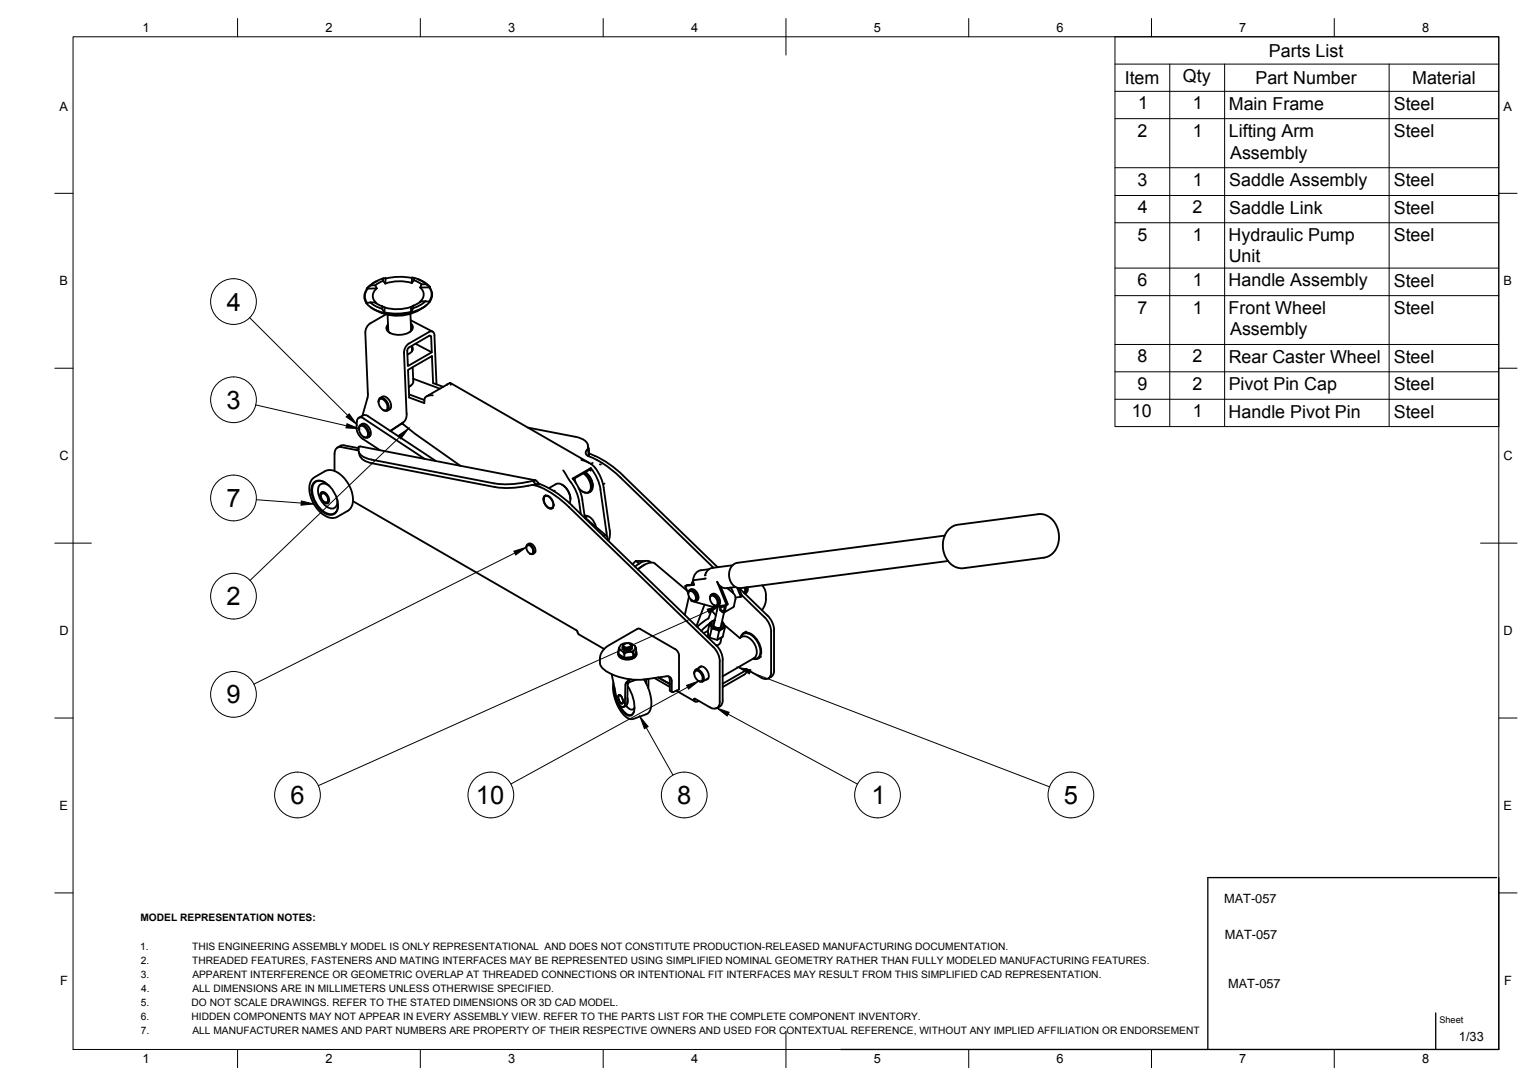
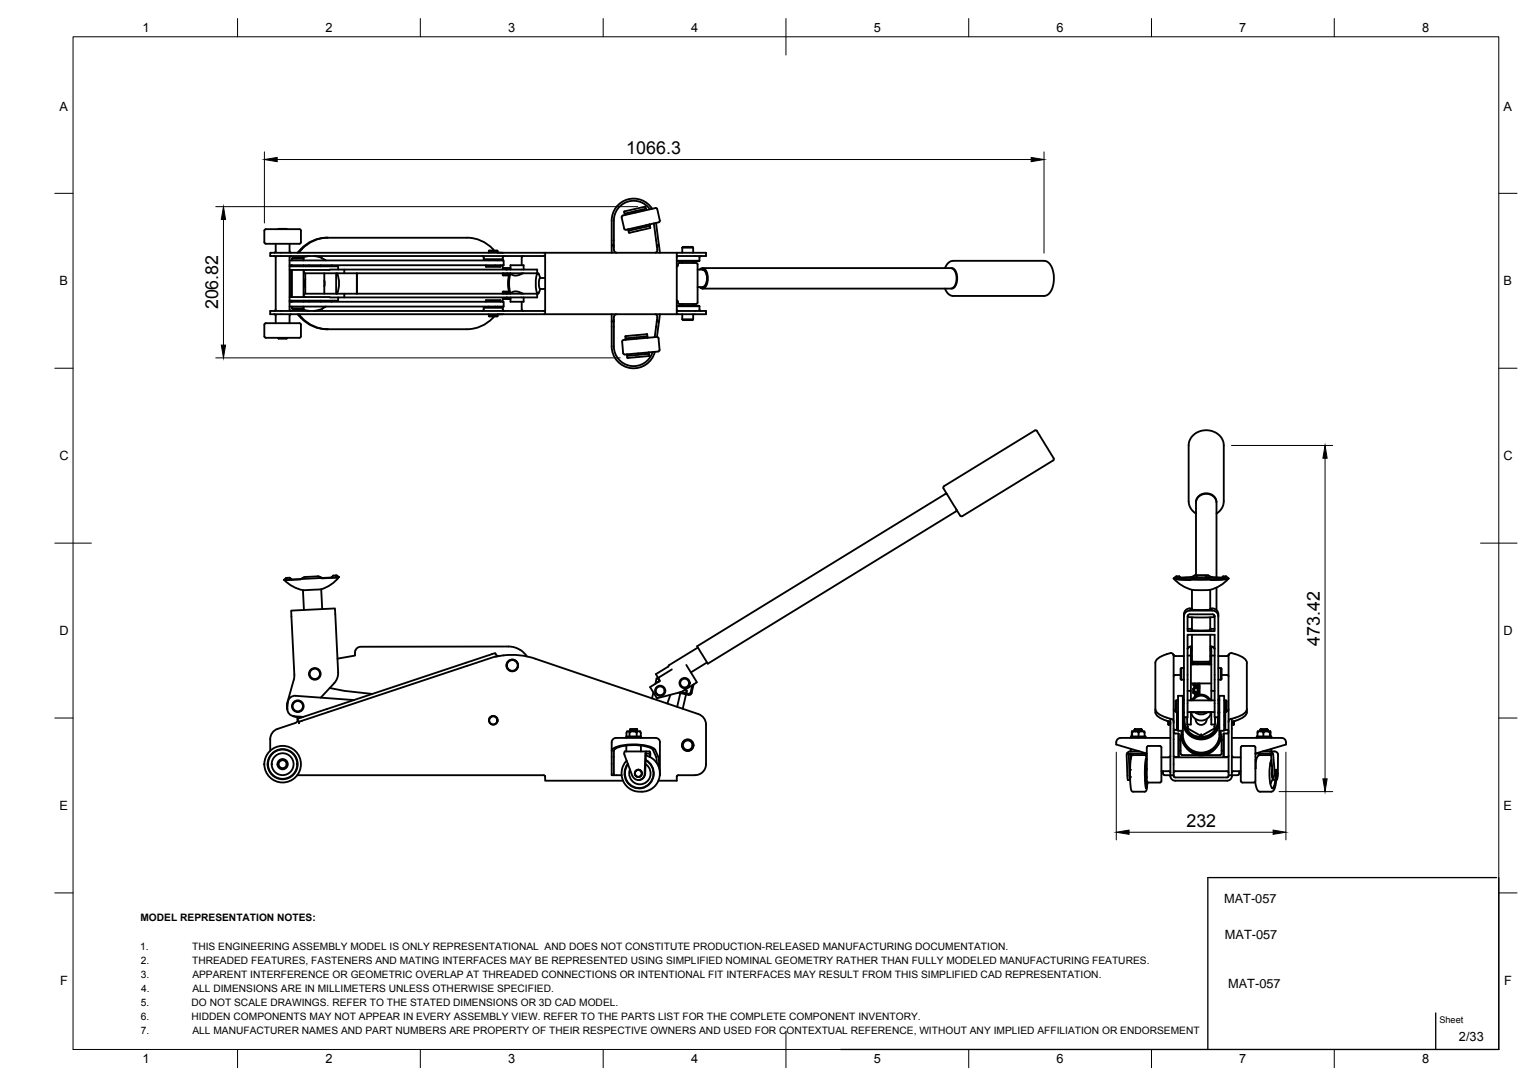
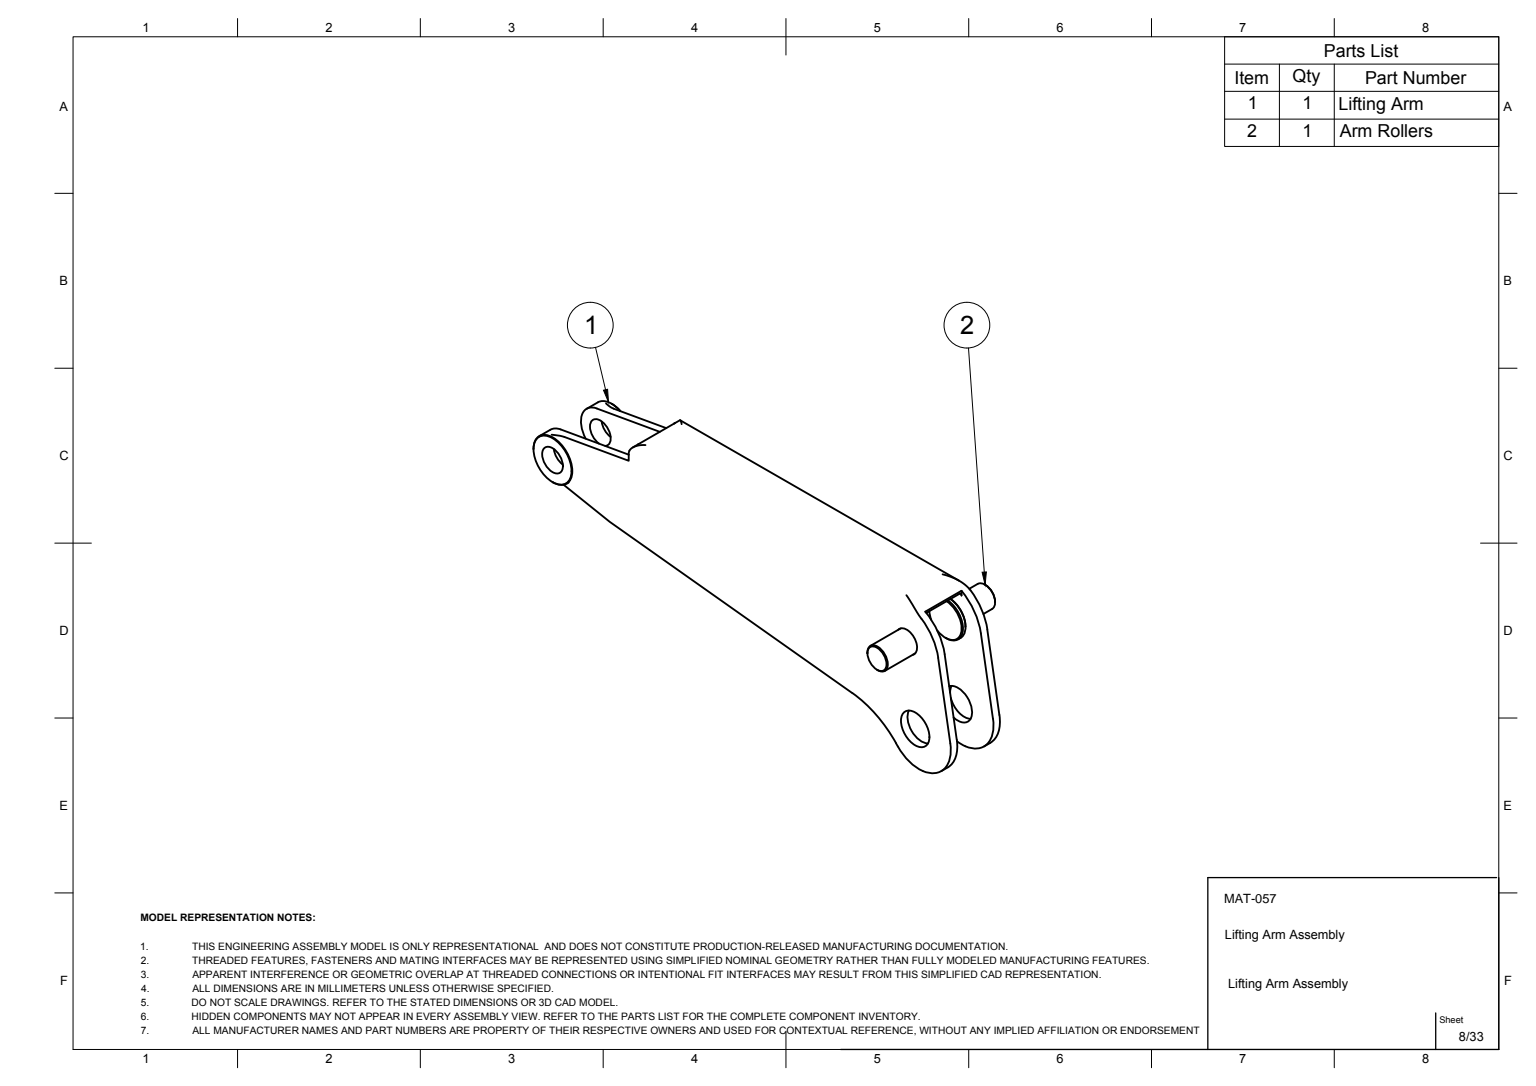
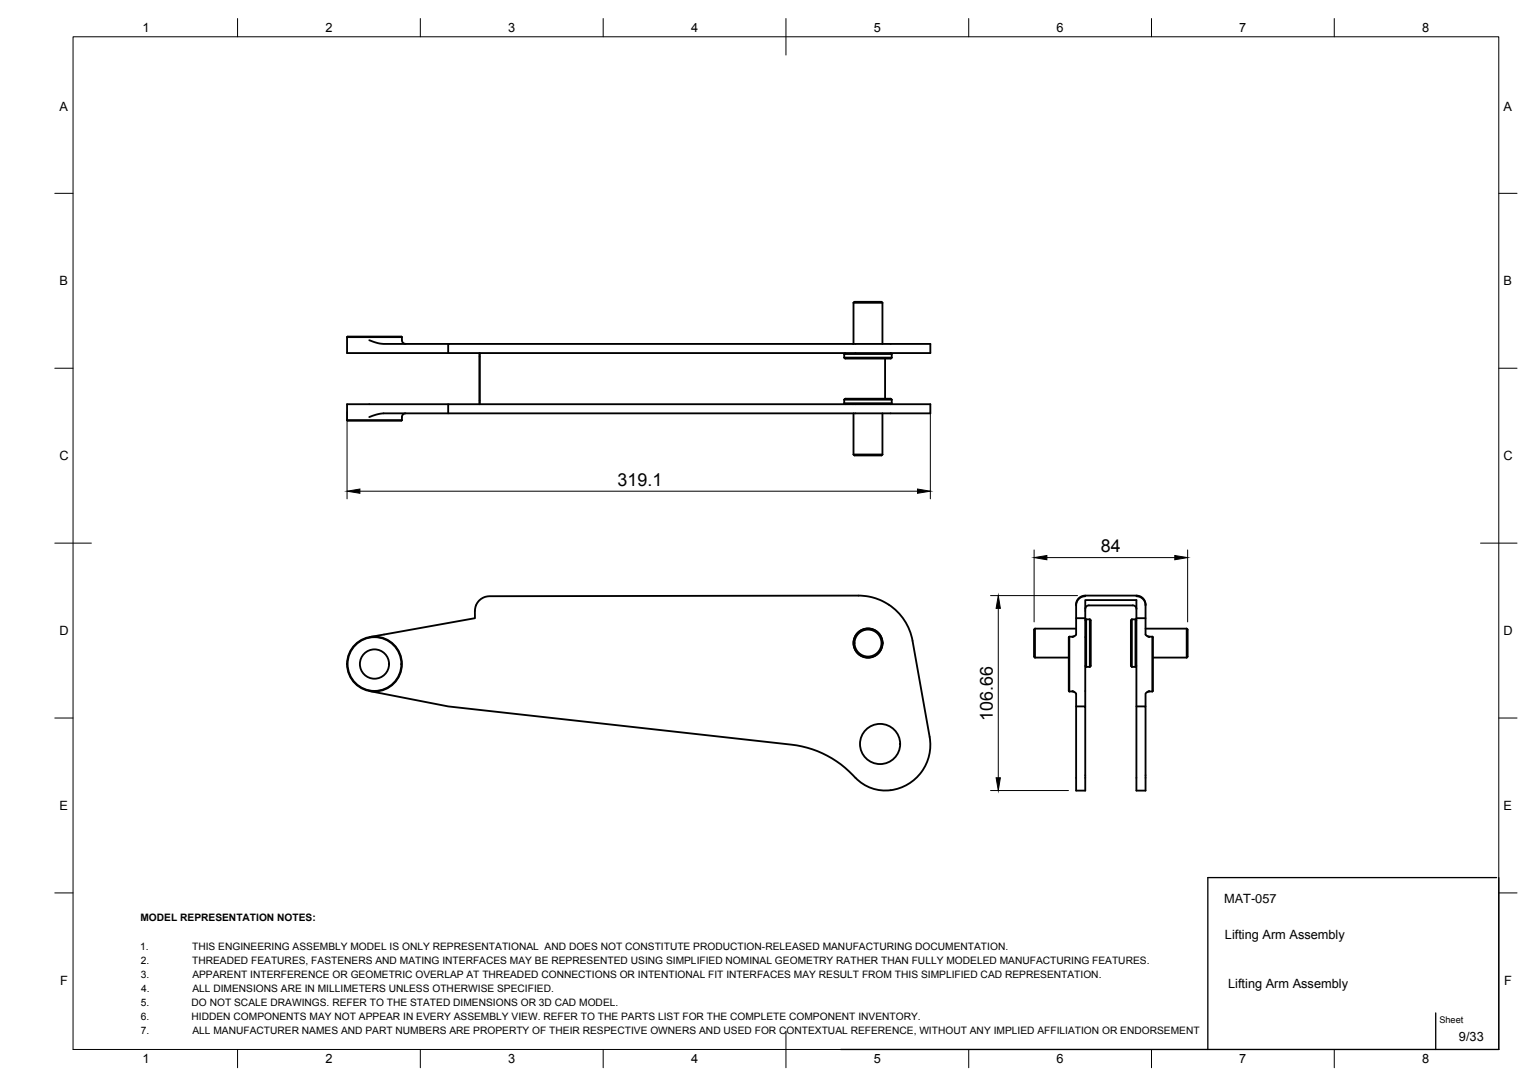
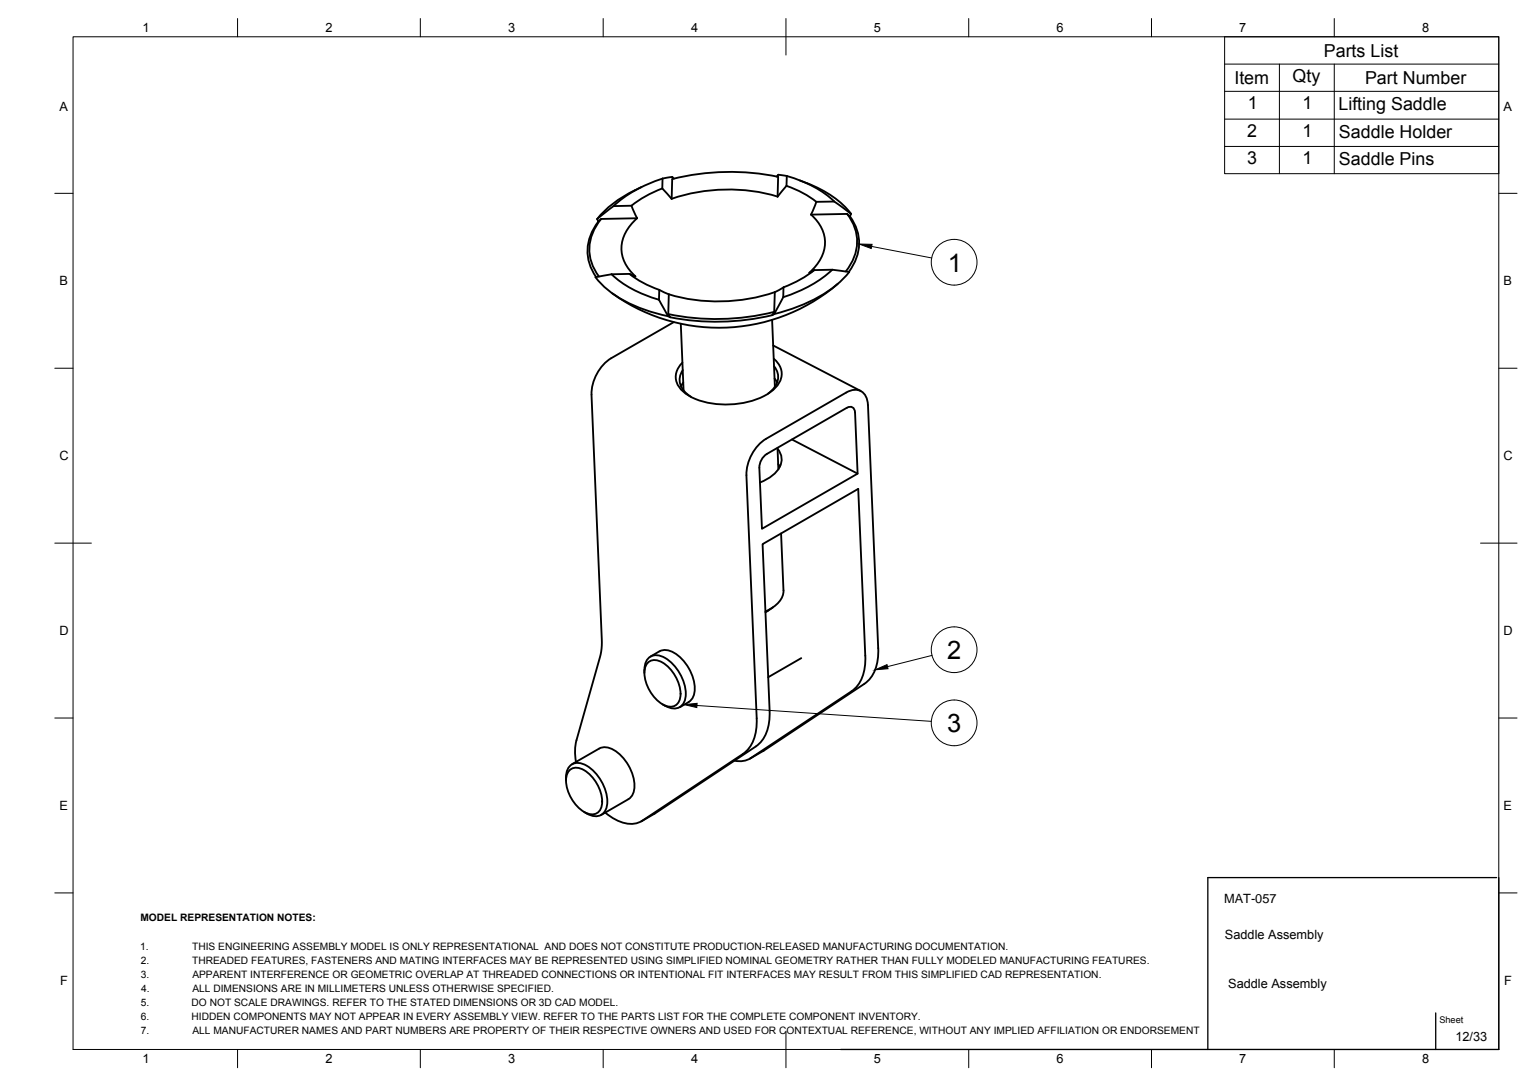
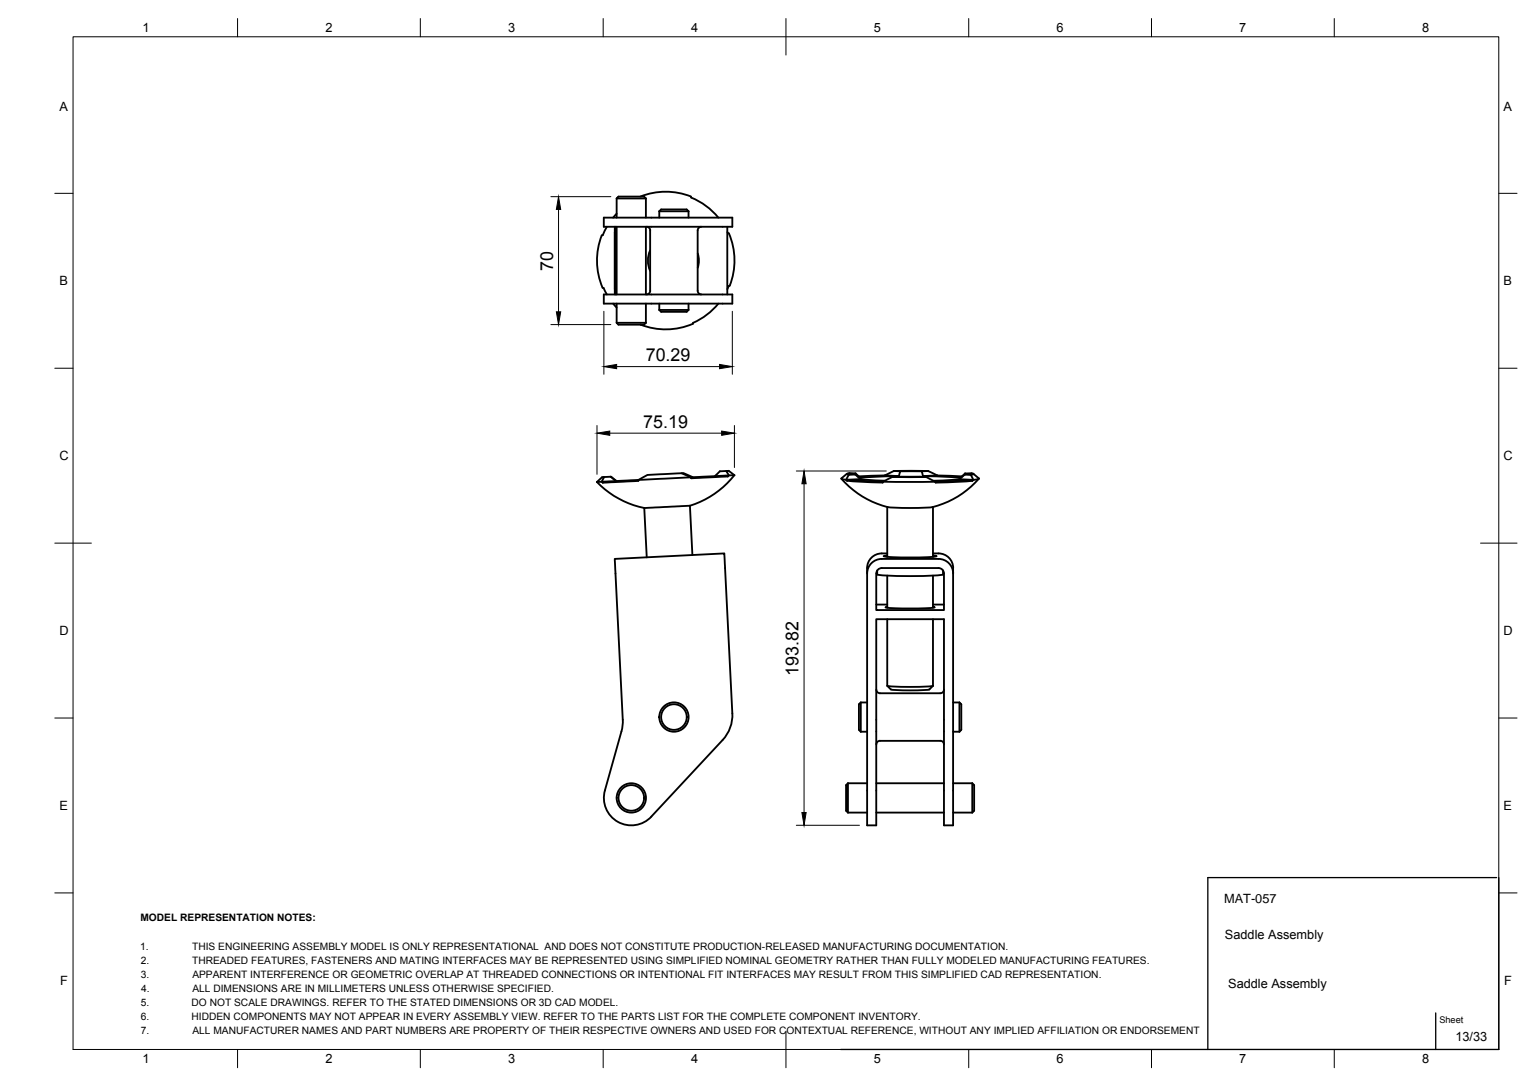
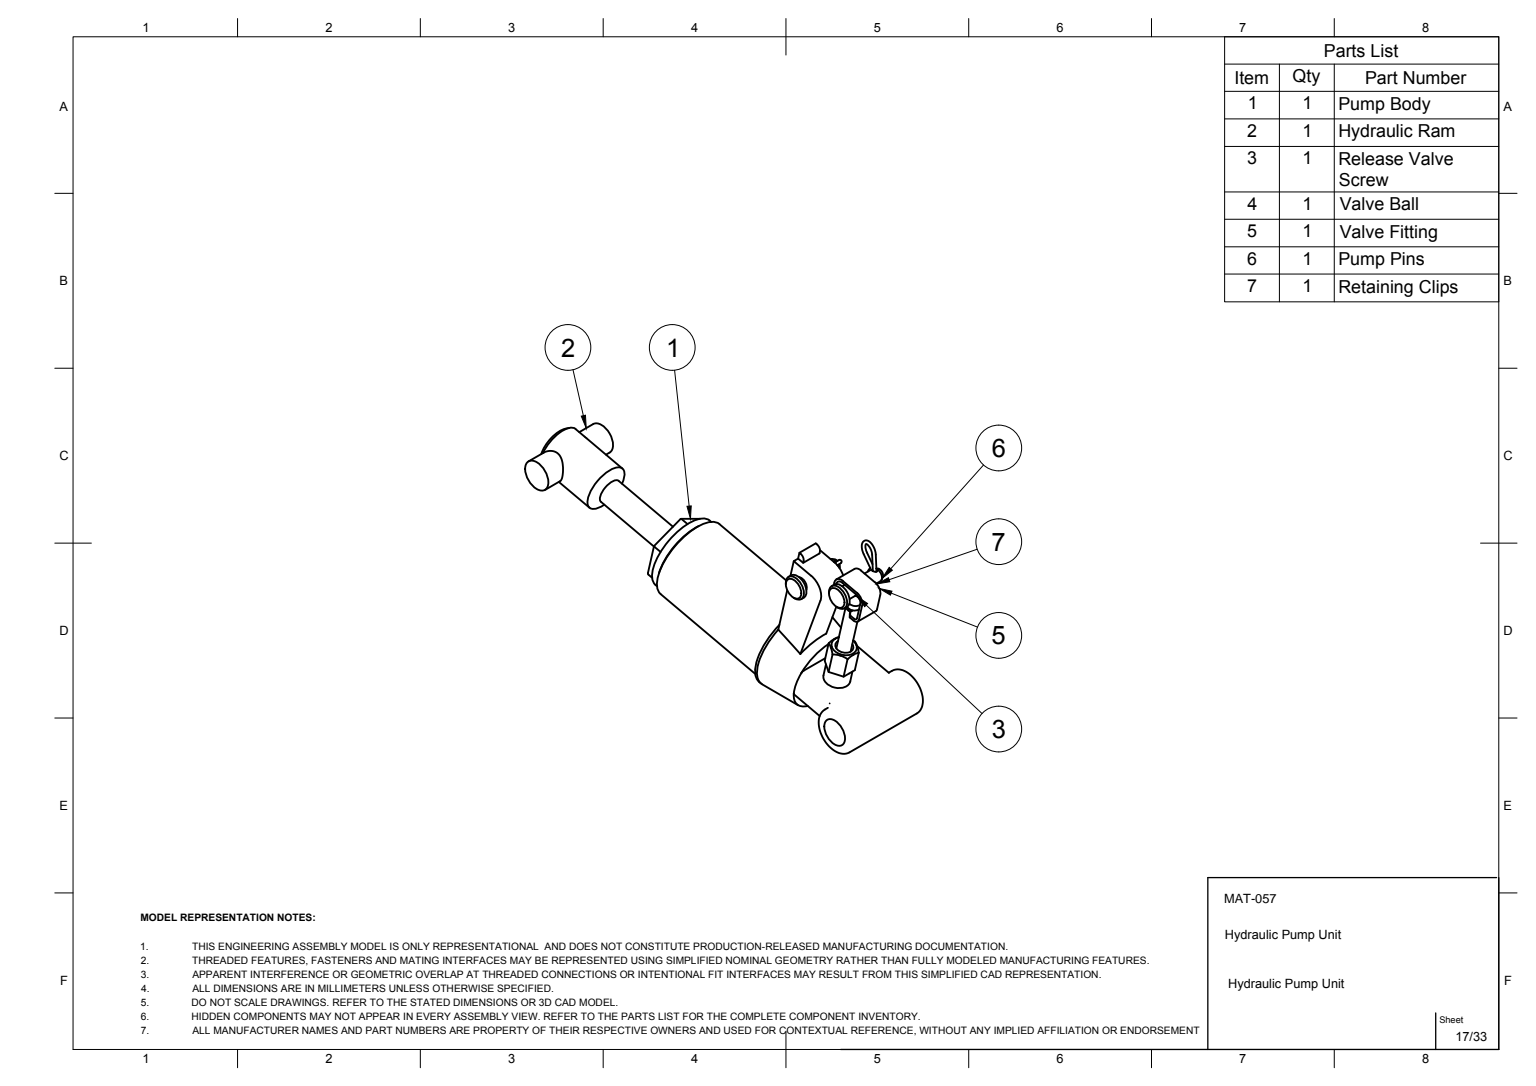
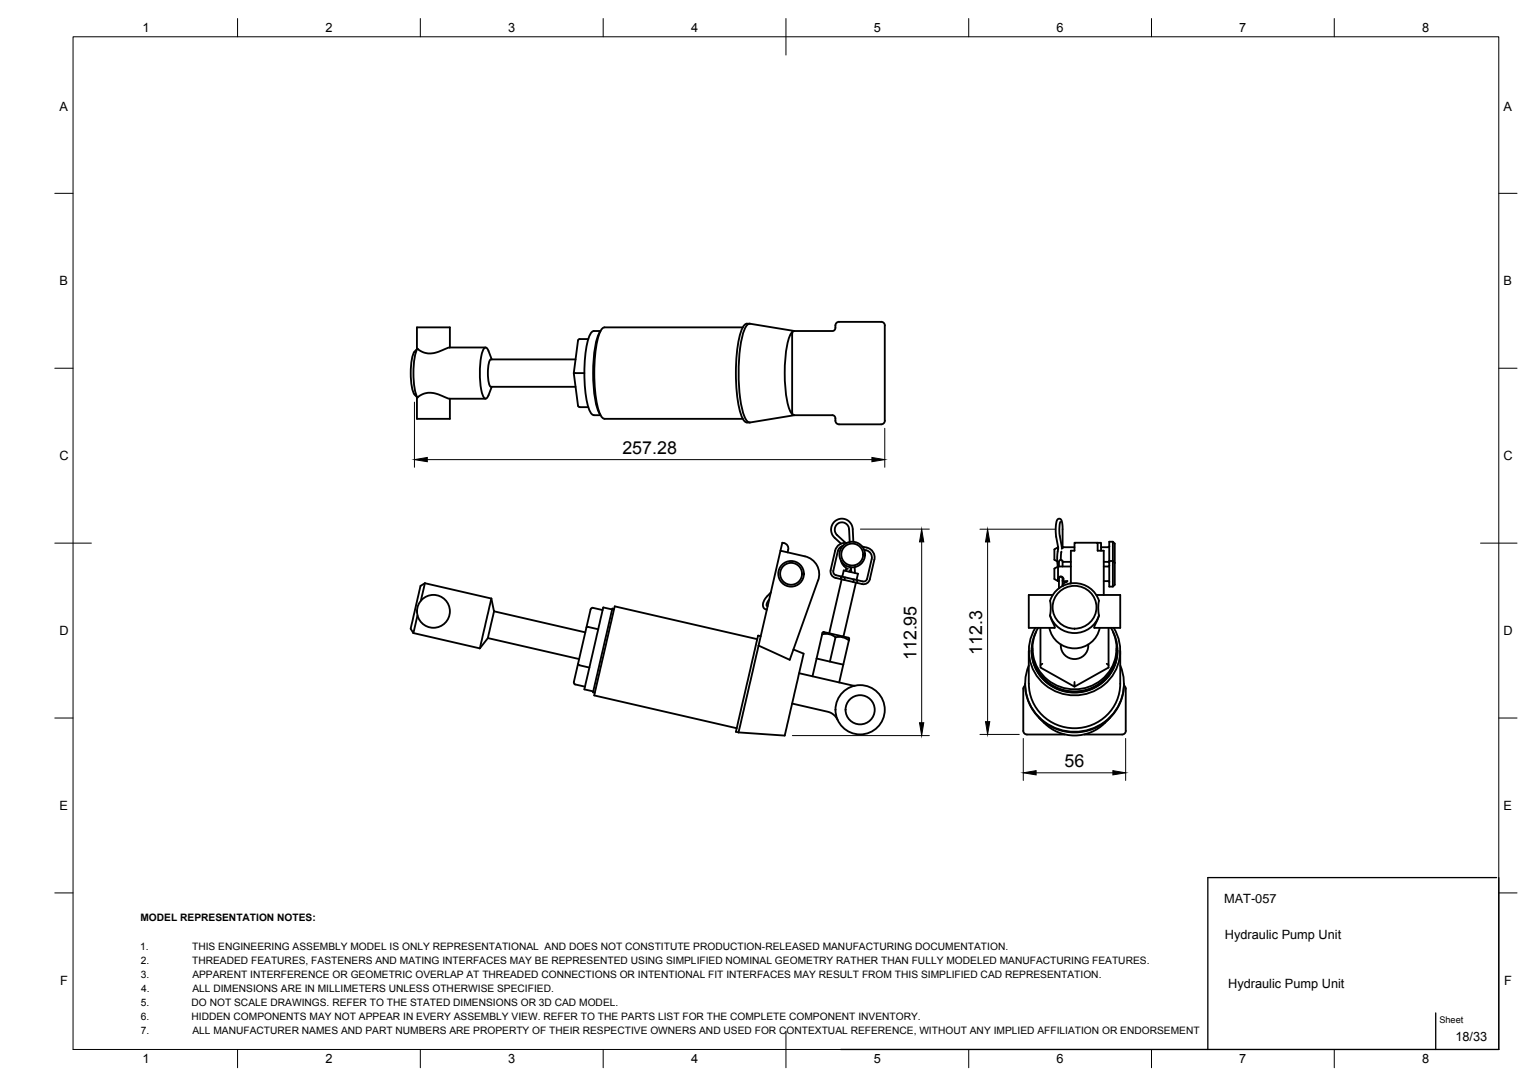
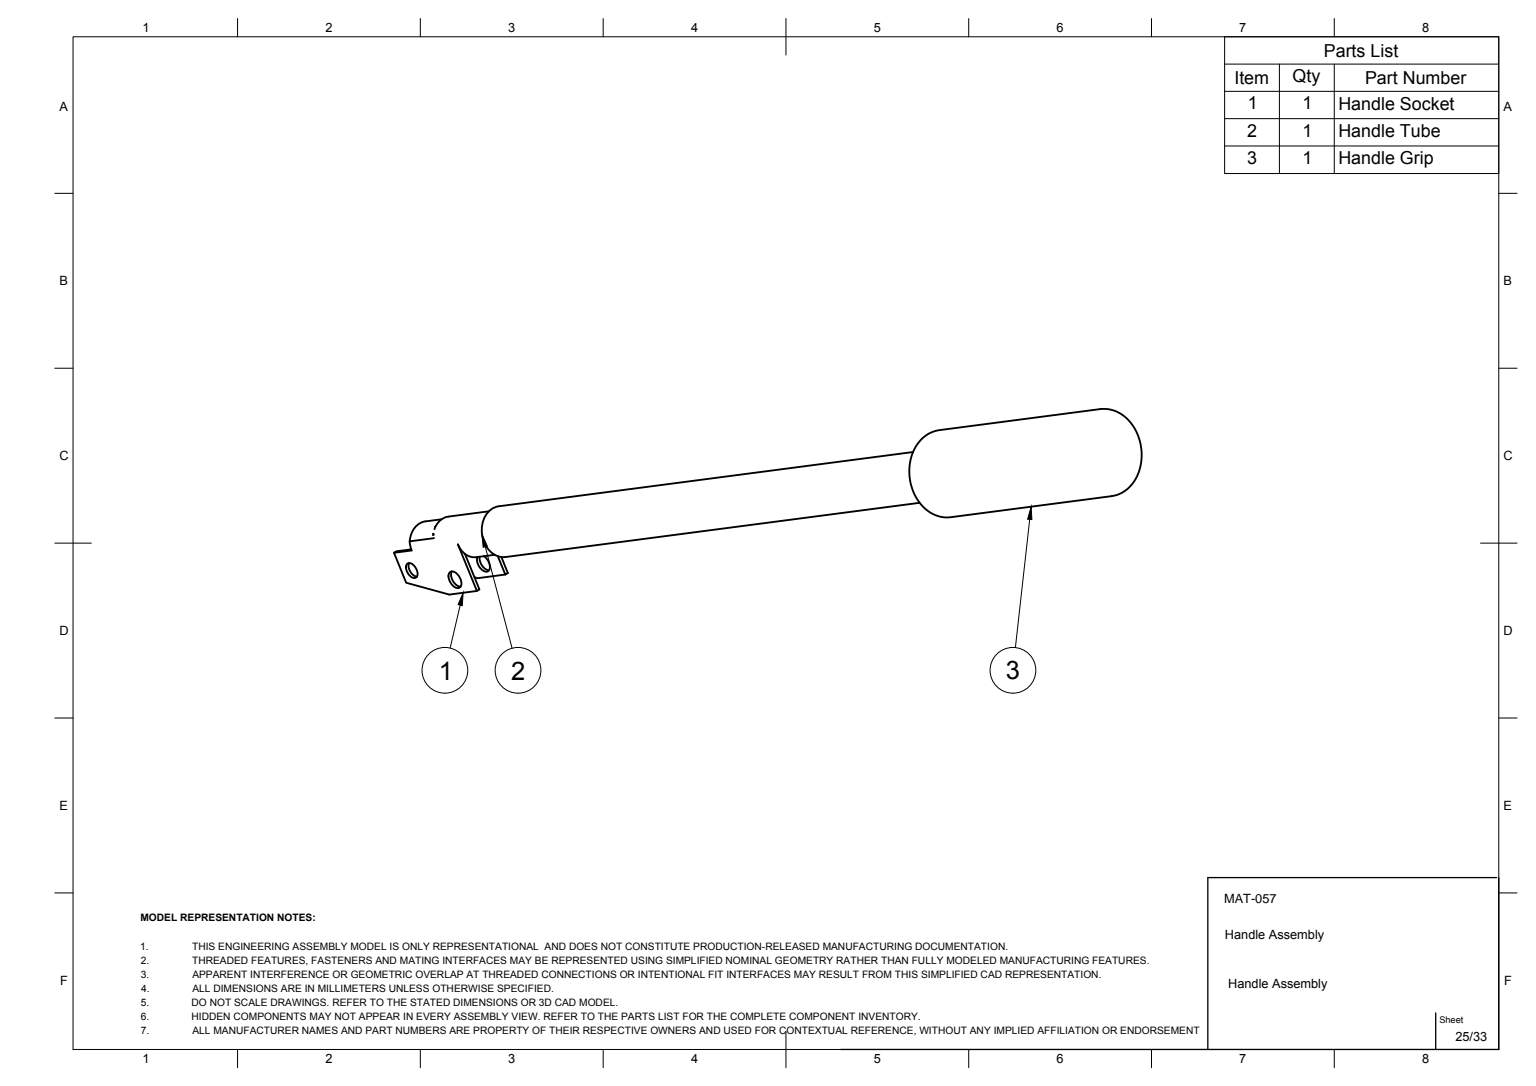
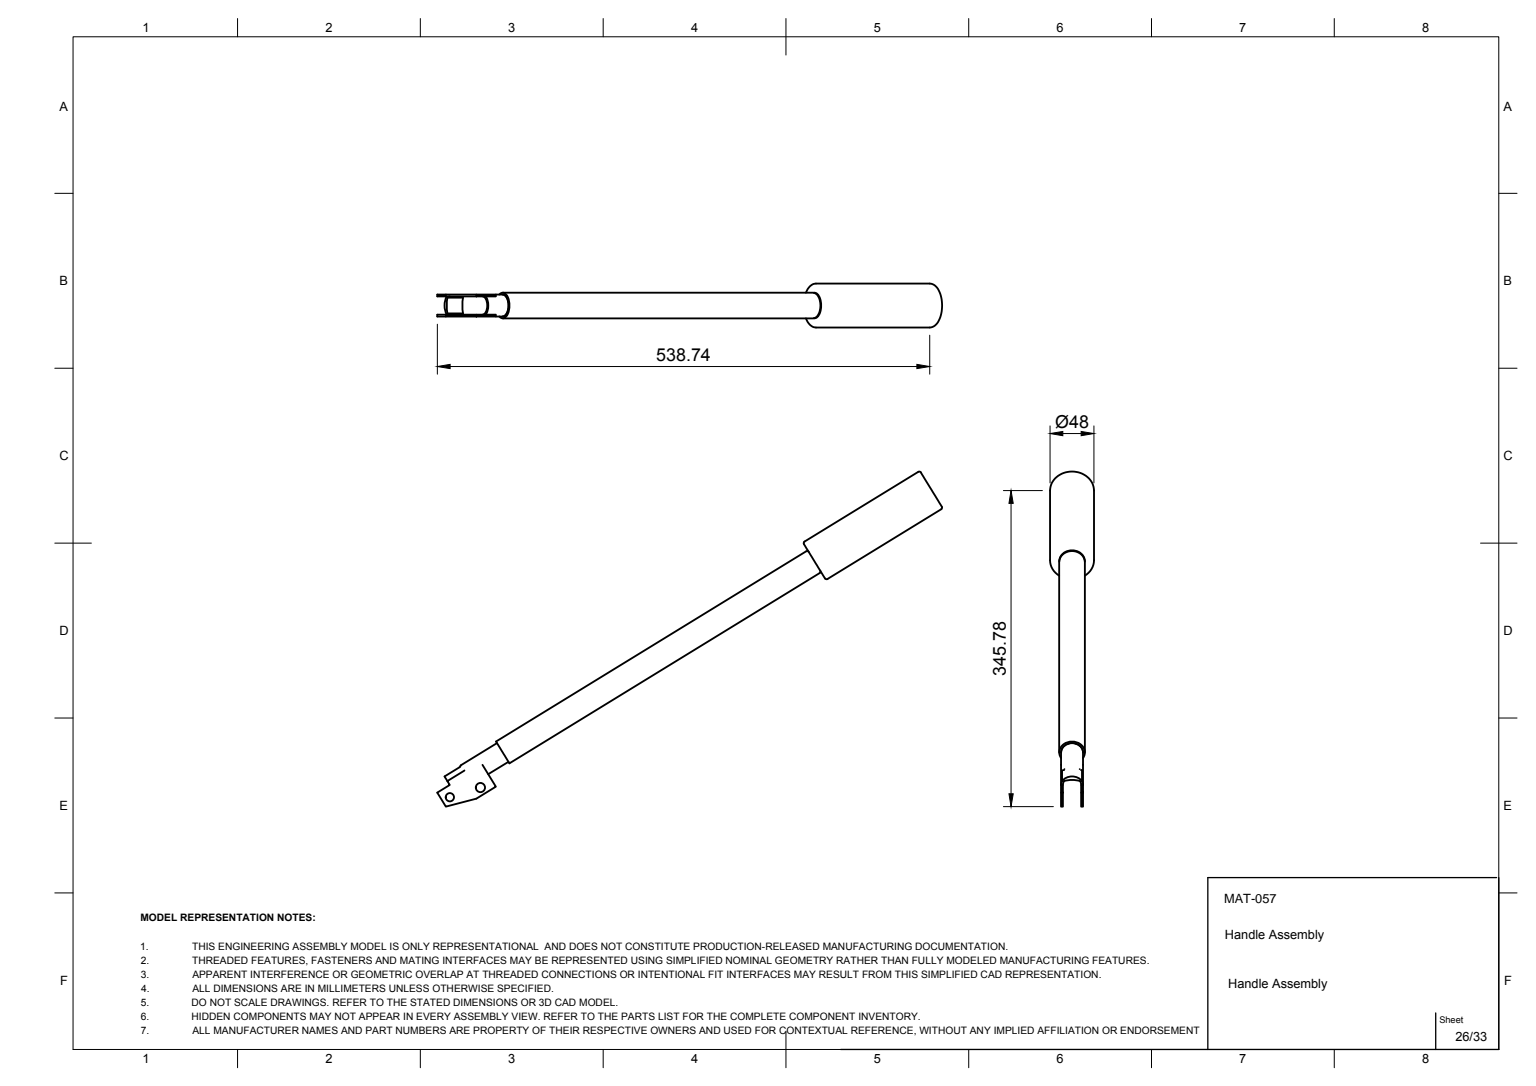
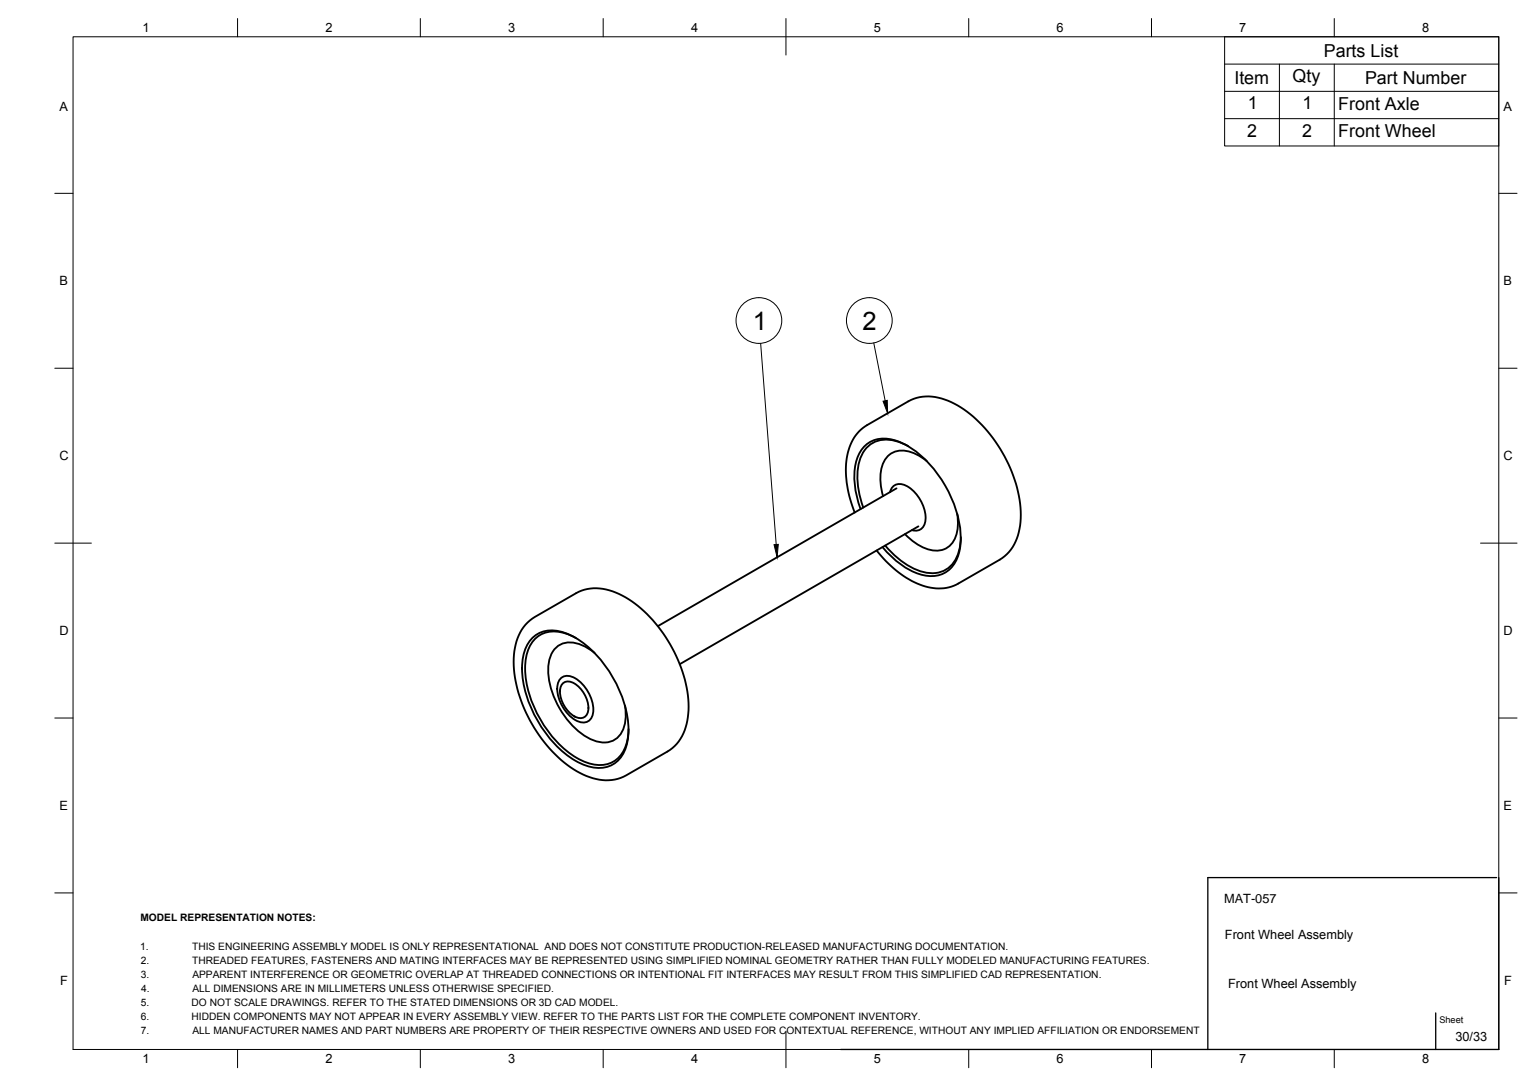
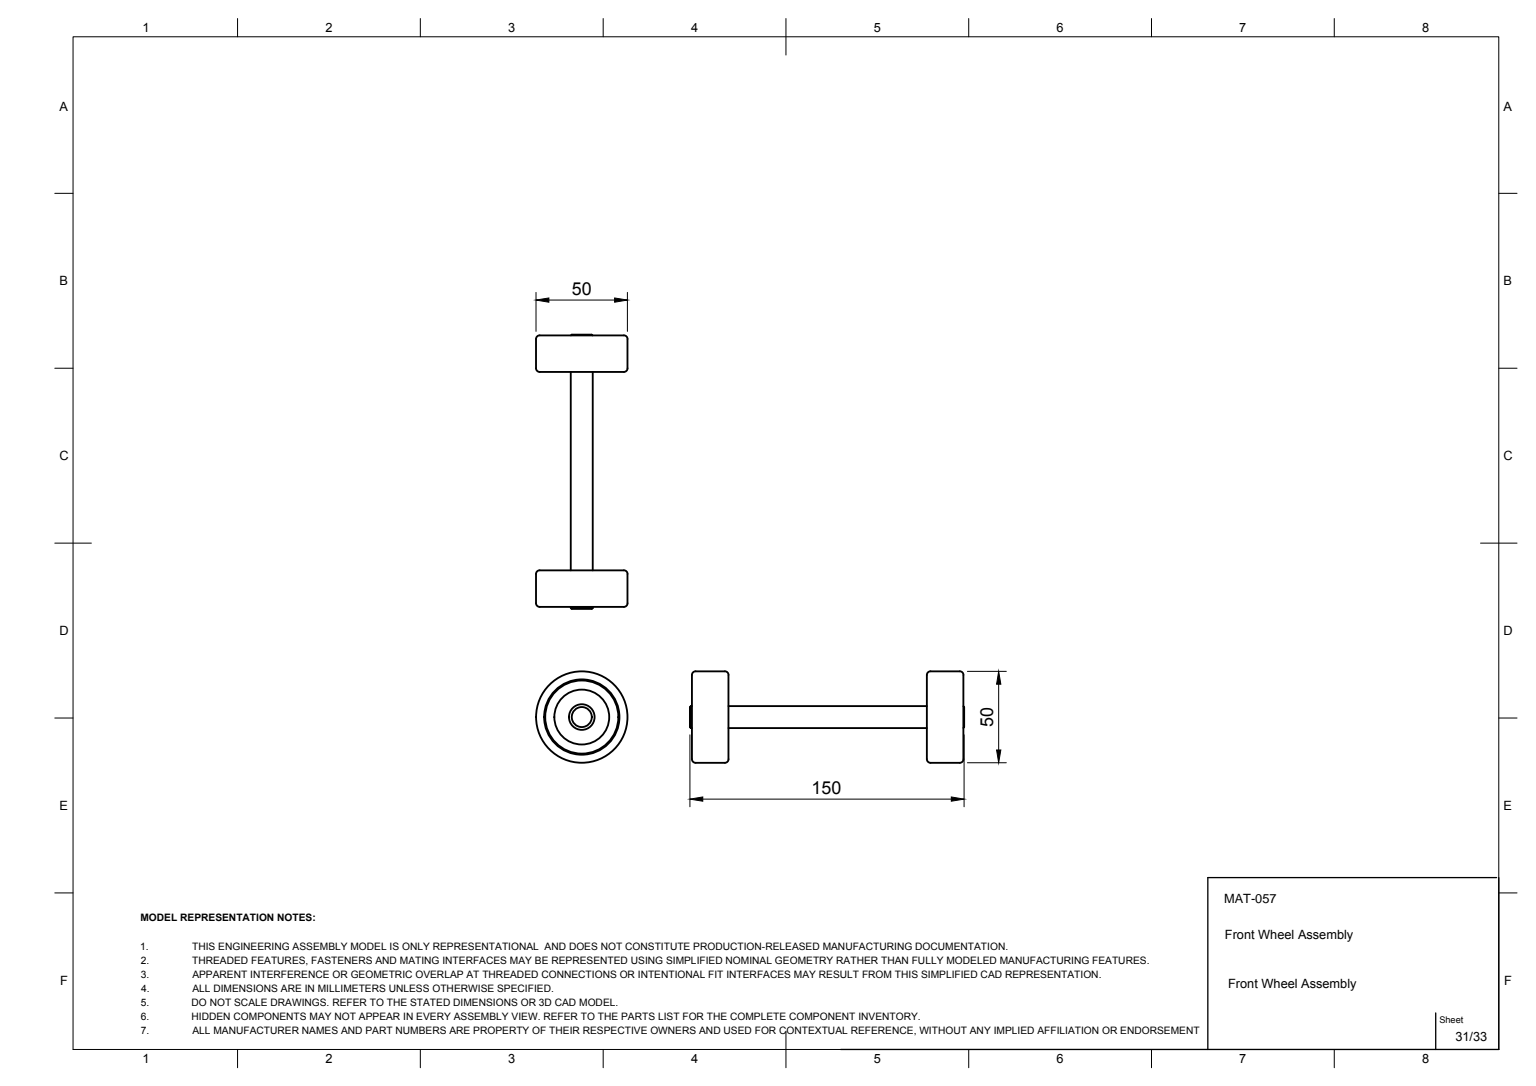
ISO-10303-21;
HEADER;
/* Generated by software containing ST-Developer
 * from STEP Tools, Inc. (www.steptools.com) 
 */

FILE_DESCRIPTION(
/* description */ ('STEP AP214', 'CAx-IF Rec.Pracs.---Representation and Presentation of Product Manufa
cturing Information (PMI)---4.0---2014-10-13'),
/* implementation_level */ '2;1');

FILE_NAME(
/* name */ 'MAT-057',
/* time_stamp */ '2026-10-28T23:34:22+01:00',
/* author */ (''),
/* organization */ (''),
/* preprocessor_version */ 'ST-DEVELOPER v20.2',
/* originating_system */ 'Autodesk Translation Framework v15.17.0.0',
/* authorisation */ '');

FILE_SCHEMA (('AP242_MANAGED_MODEL_BASED_3D_ENGINEERING_MIM_LF { 1 0 10303 442 2 1 4 }'));
ENDSEC;

DATA;
#10=MECHANICAL_DESIGN_GEOMETRIC_PRESENTATION_REPRESENTATION('',(#250,#251,
#252,#253,#254,#255,#256,#257,#258,#259,#260,#261,#262,#263,#264,#265,#266,
#267,#268,#269,#270,#271,#272,#273,#274,#275,#276,#277,#278),#27807);
#11=B_SPLINE_SURFACE_WITH_KNOTS('',1,3,((#21472,#21473,#21474,#21475,#21476,
#21477,#21478,#21479,#21480,#21481,#21482,#21483,#21484,#21485,#21486,#21487,
#21488,#21489),(#21490,#21491,#21492,#21493,#21494,#21495,#21496,#21497,
#21498,#21499,#21500,#21501,#21502,#21503,#21504,#21505,#21506,#21507)),
 .UNSPECIFIED.,.F.,.T.,.F.,(2,2),(4,2,2,2,2,2,2,2,4),(-5.33401314790998E-5,
1.0071581353373),(-0.00941606787651008,-0.00822939788115615,-0.00704272788580222,
-0.00585605789044829,-0.00466938789509436,-0.00348271789974043,-0.0022960479043865,
-0.00110937790903257,7.72920863213594E-5),.UNSPECIFIED.);
#12=B_SPLINE_SURFACE_WITH_KNOTS('',1,3,((#21574,#21575,#21576,#21577,#21578,
#21579,#21580,#21581,#21582,#21583,#21584,#21585,#21586,#21587,#21588,#21589,
#21590,#21591),(#21592,#21593,#21594,#21595,#21596,#21597,#21598,#21599,
#21600,#21601,#21602,#21603,#21604,#21605,#21606,#21607,#21608,#21609)),
 .UNSPECIFIED.,.F.,.T.,.F.,(2,2),(4,2,2,2,2,2,2,2,4),(-5.33401315292344E-5,
1.00729193620298),(-0.00941606787651008,-0.00822939788115615,-0.00704272788580222,
-0.00585605789044829,-0.00466938789509436,-0.00348271789974043,-0.0022960479043865,
-0.00110937790903257,7.72920863213577E-5),.UNSPECIFIED.);
#13=B_SPLINE_SURFACE_WITH_KNOTS('',1,3,((#21829,#21830,#21831,#21832,#21833,
#21834,#21835,#21836,#21837,#21838,#21839,#21840,#21841,#21842,#21843,#21844,
#21845,#21846),(#21847,#21848,#21849,#21850,#21851,#21852,#21853,#21854,
#21855,#21856,#21857,#21858,#21859,#21860,#21861,#21862,#21863,#21864)),
 .UNSPECIFIED.,.F.,.T.,.F.,(2,2),(4,2,2,2,2,2,2,2,4),(-4.93053323705934E-5,
1.01004399172031),(-0.00941606787651008,-0.00822939788115615,-0.00704272788580222,
-0.00585605789044829,-0.00466938789509436,-0.00348271789974043,-0.0022960479043865,
-0.00110937790903257,7.72920863213577E-5),.UNSPECIFIED.);
#14=B_SPLINE_SURFACE_WITH_KNOTS('',1,3,((#21865,#21866,#21867,#21868,#21869,
#21870,#21871,#21872,#21873,#21874,#21875,#21876,#21877,#21878,#21879,#21880,
#21881,#21882),(#21883,#21884,#21885,#21886,#21887,#21888,#21889,#21890,
#21891,#21892,#21893,#21894,#21895,#21896,#21897,#21898,#21899,#21900)),
 .UNSPECIFIED.,.F.,.T.,.F.,(2,2),(4,2,2,2,2,2,2,2,4),(-4.93053323625481E-5,
1.01010892051971),(-0.00941606787651008,-0.00822939788115615,-0.00704272788580222,
-0.00585605789044829,-0.00466938789509436,-0.00348271789974043,-0.0022960479043865,
-0.00110937790903257,7.72920863213594E-5),.UNSPECIFIED.);
#15=B_SPLINE_SURFACE_WITH_KNOTS('',1,3,((#21901,#21902,#21903,#21904,#21905,
#21906,#21907,#21908,#21909,#21910,#21911,#21912,#21913,#21914,#21915,#21916,
#21917,#21918),(#21919,#21920,#21921,#21922,#21923,#21924,#21925,#21926,
#21927,#21928,#21929,#21930,#21931,#21932,#21933,#21934,#21935,#21936)),
 .UNSPECIFIED.,.F.,.T.,.F.,(2,2),(4,2,2,2,2,2,2,2,4),(-4.62400267622051E-5,
1.00715813533735),(-0.00941606787651008,-0.00822939788115615,-0.00704272788580222,
-0.00585605789044829,-0.00466938789509436,-0.00348271789974043,-0.0022960479043865,
-0.00110937790903257,7.72920863213594E-5),.UNSPECIFIED.);
#16=B_SPLINE_SURFACE_WITH_KNOTS('',1,3,((#22003,#22004,#22005,#22006,#22007,
#22008,#22009,#22010,#22011,#22012,#22013,#22014,#22015,#22016,#22017,#22018,
#22019,#22020),(#22021,#22022,#22023,#22024,#22025,#22026,#22027,#22028,
#22029,#22030,#22031,#22032,#22033,#22034,#22035,#22036,#22037,#22038)),
 .UNSPECIFIED.,.F.,.T.,.F.,(2,2),(4,2,2,2,2,2,2,2,4),(-4.62400267636951E-5,
1.00729193620287),(-0.00941606787651008,-0.00822939788115615,-0.00704272788580222,
-0.00585605789044829,-0.00466938789509436,-0.00348271789974043,-0.0022960479043865,
-0.00110937790903257,7.72920863213577E-5),.UNSPECIFIED.);
#17=B_SPLINE_SURFACE_WITH_KNOTS('',1,3,((#22258,#22259,#22260,#22261,#22262,
#22263,#22264,#22265,#22266,#22267,#22268,#22269,#22270,#22271,#22272,#22273,
#22274,#22275),(#22276,#22277,#22278,#22279,#22280,#22281,#22282,#22283,
#22284,#22285,#22286,#22287,#22288,#22289,#22290,#22291,#22292,#22293)),
 .UNSPECIFIED.,.F.,.T.,.F.,(2,2),(4,2,2,2,2,2,2,2,4),(-4.93053323759633E-5,
1.00770004007163),(-0.00941606787651008,-0.00822939788115615,-0.00704272788580222,
-0.00585605789044829,-0.00466938789509436,-0.00348271789974043,-0.0022960479043865,
-0.00110937790903257,7.72920863213577E-5),.UNSPECIFIED.);
#18=B_SPLINE_SURFACE_WITH_KNOTS('',1,3,((#22294,#22295,#22296,#22297,#22298,
#22299,#22300,#22301,#22302,#22303,#22304,#22305,#22306,#22307,#22308,#22309,
#22310,#22311),(#22312,#22313,#22314,#22315,#22316,#22317,#22318,#22319,
#22320,#22321,#22322,#22323,#22324,#22325,#22326,#22327,#22328,#22329)),
 .UNSPECIFIED.,.F.,.T.,.F.,(2,2),(4,2,2,2,2,2,2,2,4),(-4.93053323767007E-5,
1.00811188664),(-0.00941606787651008,-0.00822939788115615,-0.00704272788580222,
-0.00585605789044829,-0.00466938789509436,-0.00348271789974043,-0.0022960479043865,
-0.00110937790903257,7.72920863213594E-5),.UNSPECIFIED.);
#19=(
BOUNDED_CURVE()
B_SPLINE_CURVE(2,(#18866,#18867,#18868),.UNSPECIFIED.,.F.,.F.)
B_SPLINE_CURVE_WITH_KNOTS((3,3),(0.462320796050368,0.567966350815043),
 .UNSPECIFIED.)
CURVE()
GEOMETRIC_REPRESENTATION_ITEM()
RATIONAL_B_SPLINE_CURVE((1.,1.,1.))
REPRESENTATION_ITEM('')
);
#20=(
BOUNDED_CURVE()
B_SPLINE_CURVE(2,(#18871,#18872,#18873),.UNSPECIFIED.,.F.,.F.)
B_SPLINE_CURVE_WITH_KNOTS((3,3),(-0.506850088621986,-0.399941526123303),
 .UNSPECIFIED.)
CURVE()
GEOMETRIC_REPRESENTATION_ITEM()
RATIONAL_B_SPLINE_CURVE((1.,1.,1.))
REPRESENTATION_ITEM('')
);
#21=(
BOUNDED_CURVE()
B_SPLINE_CURVE(2,(#18943,#18944,#18945),.UNSPECIFIED.,.F.,.F.)
B_SPLINE_CURVE_WITH_KNOTS((3,3),(-1.16469188019449,-0.591849614034338),
 .UNSPECIFIED.)
CURVE()
GEOMETRIC_REPRESENTATION_ITEM()
RATIONAL_B_SPLINE_CURVE((1.00111192291213,1.0014724056847,1.00120930695841))
REPRESENTATION_ITEM('')
);
#22=(
BOUNDED_CURVE()
B_SPLINE_CURVE(2,(#18948,#18949,#18950),.UNSPECIFIED.,.F.,.F.)
B_SPLINE_CURVE_WITH_KNOTS((3,3),(-1.18185454921906,-0.605722145160145),
 .UNSPECIFIED.)
CURVE()
GEOMETRIC_REPRESENTATION_ITEM()
RATIONAL_B_SPLINE_CURVE((1.00132604672167,1.00164254091047,1.00133534531621))
REPRESENTATION_ITEM('')
);
#23=(
BOUNDED_CURVE()
B_SPLINE_CURVE(2,(#18953,#18954,#18955),.UNSPECIFIED.,.F.,.F.)
B_SPLINE_CURVE_WITH_KNOTS((3,3),(-0.946143001046764,-0.369969297191779),
 .UNSPECIFIED.)
CURVE()
GEOMETRIC_REPRESENTATION_ITEM()
RATIONAL_B_SPLINE_CURVE((1.00070944583239,1.00100518872376,1.00067763892158))
REPRESENTATION_ITEM('')
);
#24=(
BOUNDED_CURVE()
B_SPLINE_CURVE(2,(#18958,#18959,#18960),.UNSPECIFIED.,.F.,.F.)
B_SPLINE_CURVE_WITH_KNOTS((3,3),(-0.972871322664165,-0.396853569144702),
 .UNSPECIFIED.)
CURVE()
GEOMETRIC_REPRESENTATION_ITEM()
RATIONAL_B_SPLINE_CURVE((1.00068050124441,1.00100540421751,1.00070701428562))
REPRESENTATION_ITEM('')
);
#25=(
BOUNDED_CURVE()
B_SPLINE_CURVE(2,(#18963,#18964,#18965),.UNSPECIFIED.,.F.,.F.)
B_SPLINE_CURVE_WITH_KNOTS((3,3),(-0.941872789970313,-0.366965630408099),
 .UNSPECIFIED.)
CURVE()
GEOMETRIC_REPRESENTATION_ITEM()
RATIONAL_B_SPLINE_CURVE((1.00063627989739,1.00095263621267,1.00064573232675))
REPRESENTATION_ITEM('')
);
#26=(
BOUNDED_CURVE()
B_SPLINE_CURVE(2,(#18968,#18969,#18970),.UNSPECIFIED.,.F.,.F.)
B_SPLINE_CURVE_WITH_KNOTS((3,3),(-0.937693085710887,-0.362724124749258),
 .UNSPECIFIED.)
CURVE()
GEOMETRIC_REPRESENTATION_ITEM()
RATIONAL_B_SPLINE_CURVE((1.00065371087358,1.00096152079163,1.00064606496848))
REPRESENTATION_ITEM('')
);
#27=(
BOUNDED_CURVE()
B_SPLINE_CURVE(2,(#18974,#18975,#18976),.UNSPECIFIED.,.F.,.F.)
B_SPLINE_CURVE_WITH_KNOTS((3,3),(-1.17291409885218,-0.596764361726987),
 .UNSPECIFIED.)
CURVE()
GEOMETRIC_REPRESENTATION_ITEM()
RATIONAL_B_SPLINE_CURVE((1.00133527889567,1.00164217359151,1.00132537873593))
REPRESENTATION_ITEM('')
);
#28=(
BOUNDED_CURVE()
B_SPLINE_CURVE(2,(#18979,#18980,#18981),.UNSPECIFIED.,.F.,.F.)
B_SPLINE_CURVE_WITH_KNOTS((3,3),(-1.0750860439484,-0.50223001899858),
 .UNSPECIFIED.)
CURVE()
GEOMETRIC_REPRESENTATION_ITEM()
RATIONAL_B_SPLINE_CURVE((1.00120779728153,1.00147115277612,1.00111092752705))
REPRESENTATION_ITEM('')
);
#29=(
BOUNDED_CURVE()
B_SPLINE_CURVE(2,(#18990,#18991,#18992),.UNSPECIFIED.,.F.,.F.)
B_SPLINE_CURVE_WITH_KNOTS((3,3),(0.837657703679305,0.944563738178637),
 .UNSPECIFIED.)
CURVE()
GEOMETRIC_REPRESENTATION_ITEM()
RATIONAL_B_SPLINE_CURVE((1.,1.,1.))
REPRESENTATION_ITEM('')
);
#30=(
BOUNDED_CURVE()
B_SPLINE_CURVE(2,(#18995,#18996,#18997),.UNSPECIFIED.,.F.,.F.)
B_SPLINE_CURVE_WITH_KNOTS((3,3),(0.387236418043007,0.493098305093553),
 .UNSPECIFIED.)
CURVE()
GEOMETRIC_REPRESENTATION_ITEM()
RATIONAL_B_SPLINE_CURVE((1.,1.,1.))
REPRESENTATION_ITEM('')
);
#31=(
BOUNDED_CURVE()
B_SPLINE_CURVE(2,(#19002,#19003,#19004),.UNSPECIFIED.,.F.,.F.)
B_SPLINE_CURVE_WITH_KNOTS((3,3),(1.14286008392437,1.24851586608623),
 .UNSPECIFIED.)
CURVE()
GEOMETRIC_REPRESENTATION_ITEM()
RATIONAL_B_SPLINE_CURVE((1.,1.,1.))
REPRESENTATION_ITEM('')
);
#32=(
BOUNDED_CURVE()
B_SPLINE_CURVE(2,(#19008,#19009,#19010),.UNSPECIFIED.,.F.,.F.)
B_SPLINE_CURVE_WITH_KNOTS((3,3),(0.394209164646282,0.501069286795388),
 .UNSPECIFIED.)
CURVE()
GEOMETRIC_REPRESENTATION_ITEM()
RATIONAL_B_SPLINE_CURVE((1.,1.,1.))
REPRESENTATION_ITEM('')
);
#33=(
BOUNDED_CURVE()
B_SPLINE_CURVE(2,(#19024,#19025,#19026),.UNSPECIFIED.,.F.,.F.)
B_SPLINE_CURVE_WITH_KNOTS((3,3),(0.39176954416594,0.498714042529527),
 .UNSPECIFIED.)
CURVE()
GEOMETRIC_REPRESENTATION_ITEM()
RATIONAL_B_SPLINE_CURVE((1.,1.,1.))
REPRESENTATION_ITEM('')
);
#34=(
BOUNDED_CURVE()
B_SPLINE_CURVE(2,(#19032,#19033,#19034),.UNSPECIFIED.,.F.,.F.)
B_SPLINE_CURVE_WITH_KNOTS((3,3),(1.0400161958356,1.14585618521608),
 .UNSPECIFIED.)
CURVE()
GEOMETRIC_REPRESENTATION_ITEM()
RATIONAL_B_SPLINE_CURVE((1.,1.,1.))
REPRESENTATION_ITEM('')
);
#35=(
BOUNDED_CURVE()
B_SPLINE_CURVE(2,(#19569,#19570,#19571),.UNSPECIFIED.,.F.,.F.)
B_SPLINE_CURVE_WITH_KNOTS((3,3),(3.35159796330511,5.11240655080017),
 .UNSPECIFIED.)
CURVE()
GEOMETRIC_REPRESENTATION_ITEM()
RATIONAL_B_SPLINE_CURVE((1.02178867577785,1.02219740253536,1.01702175780134))
REPRESENTATION_ITEM('')
);
#36=(
BOUNDED_CURVE()
B_SPLINE_CURVE(2,(#23410,#23411,#23412,#23413,#23414,#23415,#23416,#23417,
#23418),.UNSPECIFIED.,.F.,.F.)
B_SPLINE_CURVE_WITH_KNOTS((3,2,2,2,3),(0.964285714285714,0.973214285714286,
0.982142857142857,0.991071428571429,1.),.UNSPECIFIED.)
CURVE()
GEOMETRIC_REPRESENTATION_ITEM()
RATIONAL_B_SPLINE_CURVE((1.,0.923879532511287,1.,0.923879532511287,1.,0.923879532511287,
1.,0.923879532511287,1.))
REPRESENTATION_ITEM('')
);
#37=(
BOUNDED_CURVE()
B_SPLINE_CURVE(2,(#23421,#23422,#23423,#23424,#23425,#23426,#23427,#23428,
#23429),.UNSPECIFIED.,.F.,.F.)
B_SPLINE_CURVE_WITH_KNOTS((3,2,2,2,3),(0.964285714285714,0.973214285714286,
0.982142857142857,0.991071428571429,1.),.UNSPECIFIED.)
CURVE()
GEOMETRIC_REPRESENTATION_ITEM()
RATIONAL_B_SPLINE_CURVE((1.,0.923879532511287,1.,0.923879532511287,1.,0.923879532511287,
1.,0.923879532511287,1.))
REPRESENTATION_ITEM('')
);
#38=(
BOUNDED_CURVE()
B_SPLINE_CURVE(2,(#23434,#23435,#23436,#23437,#23438,#23439,#23440,#23441,
#23442,#23443,#23444,#23445,#23446,#23447,#23448,#23449,#23450),
 .UNSPECIFIED.,.F.,.F.)
B_SPLINE_CURVE_WITH_KNOTS((3,2,2,2,2,2,2,2,3),(0.892857142857143,0.901785714285714,
0.910714285714286,0.919642857142857,0.928571428571429,0.9375,0.946428571428571,
0.955357142857143,0.964285714285714),.UNSPECIFIED.)
CURVE()
GEOMETRIC_REPRESENTATION_ITEM()
RATIONAL_B_SPLINE_CURVE((1.,0.923879532511287,1.,0.923879532511287,1.,0.923879532511287,
1.,0.923879532511287,1.,0.923879532511287,1.,0.923879532511287,1.,0.923879532511287,
1.,0.923879532511287,1.))
REPRESENTATION_ITEM('')
);
#39=(
BOUNDED_CURVE()
B_SPLINE_CURVE(2,(#23451,#23452,#23453,#23454,#23455,#23456,#23457,#23458,
#23459,#23460,#23461,#23462,#23463,#23464,#23465,#23466,#23467),
 .UNSPECIFIED.,.F.,.F.)
B_SPLINE_CURVE_WITH_KNOTS((3,2,2,2,2,2,2,2,3),(0.892857142857143,0.901785714285714,
0.910714285714286,0.919642857142857,0.928571428571429,0.9375,0.946428571428571,
0.955357142857143,0.964285714285714),.UNSPECIFIED.)
CURVE()
GEOMETRIC_REPRESENTATION_ITEM()
RATIONAL_B_SPLINE_CURVE((1.,0.923879532511287,1.,0.923879532511287,1.,0.923879532511287,
1.,0.923879532511287,1.,0.923879532511287,1.,0.923879532511287,1.,0.923879532511287,
1.,0.923879532511287,1.))
REPRESENTATION_ITEM('')
);
#40=(
BOUNDED_CURVE()
B_SPLINE_CURVE(2,(#23472,#23473,#23474,#23475,#23476,#23477,#23478,#23479,
#23480,#23481,#23482,#23483,#23484,#23485,#23486,#23487,#23488),
 .UNSPECIFIED.,.F.,.F.)
B_SPLINE_CURVE_WITH_KNOTS((3,2,2,2,2,2,2,2,3),(0.821428571428571,0.830357142857143,
0.839285714285714,0.848214285714286,0.857142857142857,0.866071428571429,
0.875,0.883928571428571,0.892857142857143),.UNSPECIFIED.)
CURVE()
GEOMETRIC_REPRESENTATION_ITEM()
RATIONAL_B_SPLINE_CURVE((1.,0.923879532511287,1.,0.923879532511287,1.,0.923879532511287,
1.,0.923879532511287,1.,0.923879532511287,1.,0.923879532511287,1.,0.923879532511287,
1.,0.923879532511287,1.))
REPRESENTATION_ITEM('')
);
#41=(
BOUNDED_CURVE()
B_SPLINE_CURVE(2,(#23489,#23490,#23491,#23492,#23493,#23494,#23495,#23496,
#23497,#23498,#23499,#23500,#23501,#23502,#23503,#23504,#23505),
 .UNSPECIFIED.,.F.,.F.)
B_SPLINE_CURVE_WITH_KNOTS((3,2,2,2,2,2,2,2,3),(0.821428571428571,0.830357142857143,
0.839285714285714,0.848214285714286,0.857142857142857,0.866071428571429,
0.875,0.883928571428571,0.892857142857143),.UNSPECIFIED.)
CURVE()
GEOMETRIC_REPRESENTATION_ITEM()
RATIONAL_B_SPLINE_CURVE((1.,0.923879532511287,1.,0.923879532511287,1.,0.923879532511287,
1.,0.923879532511287,1.,0.923879532511287,1.,0.923879532511287,1.,0.923879532511287,
1.,0.923879532511287,1.))
REPRESENTATION_ITEM('')
);
#42=(
BOUNDED_CURVE()
B_SPLINE_CURVE(2,(#23510,#23511,#23512,#23513,#23514,#23515,#23516,#23517,
#23518,#23519,#23520,#23521,#23522,#23523,#23524,#23525,#23526),
 .UNSPECIFIED.,.F.,.F.)
B_SPLINE_CURVE_WITH_KNOTS((3,2,2,2,2,2,2,2,3),(0.75,0.758928571428571,0.767857142857143,
0.776785714285714,0.785714285714286,0.794642857142857,0.803571428571429,
0.8125,0.821428571428571),.UNSPECIFIED.)
CURVE()
GEOMETRIC_REPRESENTATION_ITEM()
RATIONAL_B_SPLINE_CURVE((1.,0.923879532511287,1.,0.923879532511287,1.,0.923879532511287,
1.,0.923879532511287,1.,0.923879532511287,1.,0.923879532511287,1.,0.923879532511287,
1.,0.923879532511287,1.))
REPRESENTATION_ITEM('')
);
#43=(
BOUNDED_CURVE()
B_SPLINE_CURVE(2,(#23527,#23528,#23529,#23530,#23531,#23532,#23533,#23534,
#23535,#23536,#23537,#23538,#23539,#23540,#23541,#23542,#23543),
 .UNSPECIFIED.,.F.,.F.)
B_SPLINE_CURVE_WITH_KNOTS((3,2,2,2,2,2,2,2,3),(0.75,0.758928571428571,0.767857142857143,
0.776785714285714,0.785714285714286,0.794642857142857,0.803571428571429,
0.8125,0.821428571428571),.UNSPECIFIED.)
CURVE()
GEOMETRIC_REPRESENTATION_ITEM()
RATIONAL_B_SPLINE_CURVE((1.,0.923879532511287,1.,0.923879532511287,1.,0.923879532511287,
1.,0.923879532511287,1.,0.923879532511287,1.,0.923879532511287,1.,0.923879532511287,
1.,0.923879532511287,1.))
REPRESENTATION_ITEM('')
);
#44=(
BOUNDED_CURVE()
B_SPLINE_CURVE(2,(#23548,#23549,#23550,#23551,#23552,#23553,#23554,#23555,
#23556,#23557,#23558,#23559,#23560,#23561,#23562,#23563,#23564),
 .UNSPECIFIED.,.F.,.F.)
B_SPLINE_CURVE_WITH_KNOTS((3,2,2,2,2,2,2,2,3),(0.678571428571429,0.6875,
0.696428571428571,0.705357142857143,0.714285714285714,0.723214285714286,
0.732142857142857,0.741071428571429,0.75),.UNSPECIFIED.)
CURVE()
GEOMETRIC_REPRESENTATION_ITEM()
RATIONAL_B_SPLINE_CURVE((1.,0.923879532511287,1.,0.923879532511287,1.,0.923879532511287,
1.,0.923879532511287,1.,0.923879532511287,1.,0.923879532511287,1.,0.923879532511287,
1.,0.923879532511287,1.))
REPRESENTATION_ITEM('')
);
#45=(
BOUNDED_CURVE()
B_SPLINE_CURVE(2,(#23565,#23566,#23567,#23568,#23569,#23570,#23571,#23572,
#23573,#23574,#23575,#23576,#23577,#23578,#23579,#23580,#23581),
 .UNSPECIFIED.,.F.,.F.)
B_SPLINE_CURVE_WITH_KNOTS((3,2,2,2,2,2,2,2,3),(0.678571428571428,0.6875,
0.696428571428571,0.705357142857143,0.714285714285714,0.723214285714286,
0.732142857142857,0.741071428571429,0.75),.UNSPECIFIED.)
CURVE()
GEOMETRIC_REPRESENTATION_ITEM()
RATIONAL_B_SPLINE_CURVE((1.,0.923879532511287,1.,0.923879532511287,1.,0.923879532511287,
1.,0.923879532511287,1.,0.923879532511287,1.,0.923879532511287,1.,0.923879532511287,
1.,0.923879532511287,1.))
REPRESENTATION_ITEM('')
);
#46=(
BOUNDED_CURVE()
B_SPLINE_CURVE(2,(#23586,#23587,#23588,#23589,#23590,#23591,#23592,#23593,
#23594,#23595,#23596,#23597,#23598,#23599,#23600,#23601,#23602),
 .UNSPECIFIED.,.F.,.F.)
B_SPLINE_CURVE_WITH_KNOTS((3,2,2,2,2,2,2,2,3),(0.607142857142857,0.616071428571429,
0.625,0.633928571428571,0.642857142857143,0.651785714285714,0.660714285714286,
0.669642857142857,0.678571428571429),.UNSPECIFIED.)
CURVE()
GEOMETRIC_REPRESENTATION_ITEM()
RATIONAL_B_SPLINE_CURVE((1.,0.923879532511287,1.,0.923879532511287,1.,0.923879532511287,
1.,0.923879532511287,1.,0.923879532511287,1.,0.923879532511287,1.,0.923879532511287,
1.,0.923879532511287,1.))
REPRESENTATION_ITEM('')
);
#47=(
BOUNDED_CURVE()
B_SPLINE_CURVE(2,(#23603,#23604,#23605,#23606,#23607,#23608,#23609,#23610,
#23611,#23612,#23613,#23614,#23615,#23616,#23617,#23618,#23619),
 .UNSPECIFIED.,.F.,.F.)
B_SPLINE_CURVE_WITH_KNOTS((3,2,2,2,2,2,2,2,3),(0.607142857142857,0.616071428571429,
0.625,0.633928571428571,0.642857142857143,0.651785714285714,0.660714285714286,
0.669642857142857,0.678571428571428),.UNSPECIFIED.)
CURVE()
GEOMETRIC_REPRESENTATION_ITEM()
RATIONAL_B_SPLINE_CURVE((1.,0.923879532511287,1.,0.923879532511287,1.,0.923879532511287,
1.,0.923879532511287,1.,0.923879532511287,1.,0.923879532511287,1.,0.923879532511287,
1.,0.923879532511287,1.))
REPRESENTATION_ITEM('')
);
#48=(
BOUNDED_CURVE()
B_SPLINE_CURVE(2,(#23624,#23625,#23626,#23627,#23628,#23629,#23630,#23631,
#23632,#23633,#23634,#23635,#23636,#23637,#23638,#23639,#23640),
 .UNSPECIFIED.,.F.,.F.)
B_SPLINE_CURVE_WITH_KNOTS((3,2,2,2,2,2,2,2,3),(0.535714285714286,0.544642857142857,
0.553571428571429,0.5625,0.571428571428571,0.580357142857143,0.589285714285714,
0.598214285714286,0.607142857142857),.UNSPECIFIED.)
CURVE()
GEOMETRIC_REPRESENTATION_ITEM()
RATIONAL_B_SPLINE_CURVE((1.,0.923879532511287,1.,0.923879532511287,1.,0.923879532511287,
1.,0.923879532511287,1.,0.923879532511287,1.,0.923879532511287,1.,0.923879532511287,
1.,0.923879532511287,1.))
REPRESENTATION_ITEM('')
);
#49=(
BOUNDED_CURVE()
B_SPLINE_CURVE(2,(#23641,#23642,#23643,#23644,#23645,#23646,#23647,#23648,
#23649,#23650,#23651,#23652,#23653,#23654,#23655,#23656,#23657),
 .UNSPECIFIED.,.F.,.F.)
B_SPLINE_CURVE_WITH_KNOTS((3,2,2,2,2,2,2,2,3),(0.535714285714286,0.544642857142857,
0.553571428571429,0.5625,0.571428571428571,0.580357142857143,0.589285714285714,
0.598214285714286,0.607142857142857),.UNSPECIFIED.)
CURVE()
GEOMETRIC_REPRESENTATION_ITEM()
RATIONAL_B_SPLINE_CURVE((1.,0.923879532511287,1.,0.923879532511287,1.,0.923879532511287,
1.,0.923879532511287,1.,0.923879532511287,1.,0.923879532511287,1.,0.923879532511287,
1.,0.923879532511287,1.))
REPRESENTATION_ITEM('')
);
#50=(
BOUNDED_CURVE()
B_SPLINE_CURVE(2,(#23662,#23663,#23664,#23665,#23666,#23667,#23668,#23669,
#23670,#23671,#23672,#23673,#23674,#23675,#23676,#23677,#23678),
 .UNSPECIFIED.,.F.,.F.)
B_SPLINE_CURVE_WITH_KNOTS((3,2,2,2,2,2,2,2,3),(0.464285714285714,0.473214285714286,
0.482142857142857,0.491071428571429,0.5,0.508928571428571,0.517857142857143,
0.526785714285714,0.535714285714286),.UNSPECIFIED.)
CURVE()
GEOMETRIC_REPRESENTATION_ITEM()
RATIONAL_B_SPLINE_CURVE((1.,0.923879532511287,1.,0.923879532511287,1.,0.923879532511287,
1.,0.923879532511287,1.,0.923879532511287,1.,0.923879532511287,1.,0.923879532511287,
1.,0.923879532511287,1.))
REPRESENTATION_ITEM('')
);
#51=(
BOUNDED_CURVE()
B_SPLINE_CURVE(2,(#23679,#23680,#23681,#23682,#23683,#23684,#23685,#23686,
#23687,#23688,#23689,#23690,#23691,#23692,#23693,#23694,#23695),
 .UNSPECIFIED.,.F.,.F.)
B_SPLINE_CURVE_WITH_KNOTS((3,2,2,2,2,2,2,2,3),(0.464285714285714,0.473214285714286,
0.482142857142857,0.491071428571429,0.5,0.508928571428571,0.517857142857143,
0.526785714285714,0.535714285714286),.UNSPECIFIED.)
CURVE()
GEOMETRIC_REPRESENTATION_ITEM()
RATIONAL_B_SPLINE_CURVE((1.,0.923879532511287,1.,0.923879532511287,1.,0.923879532511287,
1.,0.923879532511287,1.,0.923879532511287,1.,0.923879532511287,1.,0.923879532511287,
1.,0.923879532511287,1.))
REPRESENTATION_ITEM('')
);
#52=(
BOUNDED_CURVE()
B_SPLINE_CURVE(2,(#23700,#23701,#23702,#23703,#23704,#23705,#23706,#23707,
#23708,#23709,#23710,#23711,#23712,#23713,#23714,#23715,#23716),
 .UNSPECIFIED.,.F.,.F.)
B_SPLINE_CURVE_WITH_KNOTS((3,2,2,2,2,2,2,2,3),(0.392857142857143,0.401785714285714,
0.410714285714286,0.419642857142857,0.428571428571429,0.4375,0.446428571428571,
0.455357142857143,0.464285714285714),.UNSPECIFIED.)
CURVE()
GEOMETRIC_REPRESENTATION_ITEM()
RATIONAL_B_SPLINE_CURVE((1.,0.923879532511287,1.,0.923879532511287,1.,0.923879532511287,
1.,0.923879532511287,1.,0.923879532511287,1.,0.923879532511287,1.,0.923879532511287,
1.,0.923879532511287,1.))
REPRESENTATION_ITEM('')
);
#53=(
BOUNDED_CURVE()
B_SPLINE_CURVE(2,(#23717,#23718,#23719,#23720,#23721,#23722,#23723,#23724,
#23725,#23726,#23727,#23728,#23729,#23730,#23731,#23732,#23733),
 .UNSPECIFIED.,.F.,.F.)
B_SPLINE_CURVE_WITH_KNOTS((3,2,2,2,2,2,2,2,3),(0.392857142857143,0.401785714285714,
0.410714285714286,0.419642857142857,0.428571428571429,0.4375,0.446428571428571,
0.455357142857143,0.464285714285714),.UNSPECIFIED.)
CURVE()
GEOMETRIC_REPRESENTATION_ITEM()
RATIONAL_B_SPLINE_CURVE((1.,0.923879532511287,1.,0.923879532511287,1.,0.923879532511287,
1.,0.923879532511287,1.,0.923879532511287,1.,0.923879532511287,1.,0.923879532511287,
1.,0.923879532511287,1.))
REPRESENTATION_ITEM('')
);
#54=(
BOUNDED_CURVE()
B_SPLINE_CURVE(2,(#23738,#23739,#23740,#23741,#23742,#23743,#23744,#23745,
#23746,#23747,#23748,#23749,#23750,#23751,#23752,#23753,#23754),
 .UNSPECIFIED.,.F.,.F.)
B_SPLINE_CURVE_WITH_KNOTS((3,2,2,2,2,2,2,2,3),(0.321428571428571,0.330357142857143,
0.339285714285714,0.348214285714286,0.357142857142857,0.366071428571429,
0.375,0.383928571428571,0.392857142857143),.UNSPECIFIED.)
CURVE()
GEOMETRIC_REPRESENTATION_ITEM()
RATIONAL_B_SPLINE_CURVE((1.,0.923879532511287,1.,0.923879532511287,1.,0.923879532511287,
1.,0.923879532511287,1.,0.923879532511287,1.,0.923879532511287,1.,0.923879532511287,
1.,0.923879532511287,1.))
REPRESENTATION_ITEM('')
);
#55=(
BOUNDED_CURVE()
B_SPLINE_CURVE(2,(#23755,#23756,#23757,#23758,#23759,#23760,#23761,#23762,
#23763,#23764,#23765,#23766,#23767,#23768,#23769,#23770,#23771),
 .UNSPECIFIED.,.F.,.F.)
B_SPLINE_CURVE_WITH_KNOTS((3,2,2,2,2,2,2,2,3),(0.321428571428571,0.330357142857143,
0.339285714285714,0.348214285714286,0.357142857142857,0.366071428571429,
0.375,0.383928571428571,0.392857142857143),.UNSPECIFIED.)
CURVE()
GEOMETRIC_REPRESENTATION_ITEM()
RATIONAL_B_SPLINE_CURVE((1.,0.923879532511287,1.,0.923879532511287,1.,0.923879532511287,
1.,0.923879532511287,1.,0.923879532511287,1.,0.923879532511287,1.,0.923879532511287,
1.,0.923879532511287,1.))
REPRESENTATION_ITEM('')
);
#56=(
BOUNDED_CURVE()
B_SPLINE_CURVE(2,(#23776,#23777,#23778,#23779,#23780,#23781,#23782,#23783,
#23784,#23785,#23786,#23787,#23788,#23789,#23790,#23791,#23792),
 .UNSPECIFIED.,.F.,.F.)
B_SPLINE_CURVE_WITH_KNOTS((3,2,2,2,2,2,2,2,3),(0.25,0.258928571428571,0.267857142857143,
0.276785714285714,0.285714285714286,0.294642857142857,0.303571428571429,
0.3125,0.321428571428571),.UNSPECIFIED.)
CURVE()
GEOMETRIC_REPRESENTATION_ITEM()
RATIONAL_B_SPLINE_CURVE((1.,0.923879532511287,1.,0.923879532511287,1.,0.923879532511287,
1.,0.923879532511287,1.,0.923879532511287,1.,0.923879532511287,1.,0.923879532511287,
1.,0.923879532511287,1.))
REPRESENTATION_ITEM('')
);
#57=(
BOUNDED_CURVE()
B_SPLINE_CURVE(2,(#23793,#23794,#23795,#23796,#23797,#23798,#23799,#23800,
#23801,#23802,#23803,#23804,#23805,#23806,#23807,#23808,#23809),
 .UNSPECIFIED.,.F.,.F.)
B_SPLINE_CURVE_WITH_KNOTS((3,2,2,2,2,2,2,2,3),(0.25,0.258928571428571,0.267857142857143,
0.276785714285714,0.285714285714286,0.294642857142857,0.303571428571429,
0.3125,0.321428571428571),.UNSPECIFIED.)
CURVE()
GEOMETRIC_REPRESENTATION_ITEM()
RATIONAL_B_SPLINE_CURVE((1.,0.923879532511287,1.,0.923879532511287,1.,0.923879532511287,
1.,0.923879532511287,1.,0.923879532511287,1.,0.923879532511287,1.,0.923879532511287,
1.,0.923879532511287,1.))
REPRESENTATION_ITEM('')
);
#58=(
BOUNDED_CURVE()
B_SPLINE_CURVE(2,(#23814,#23815,#23816,#23817,#23818,#23819,#23820,#23821,
#23822,#23823,#23824,#23825,#23826,#23827,#23828,#23829,#23830),
 .UNSPECIFIED.,.F.,.F.)
B_SPLINE_CURVE_WITH_KNOTS((3,2,2,2,2,2,2,2,3),(0.178571428571429,0.1875,
0.196428571428571,0.205357142857143,0.214285714285714,0.223214285714286,
0.232142857142857,0.241071428571429,0.25),.UNSPECIFIED.)
CURVE()
GEOMETRIC_REPRESENTATION_ITEM()
RATIONAL_B_SPLINE_CURVE((1.,0.923879532511287,1.,0.923879532511287,1.,0.923879532511287,
1.,0.923879532511287,1.,0.923879532511287,1.,0.923879532511287,1.,0.923879532511287,
1.,0.923879532511287,1.))
REPRESENTATION_ITEM('')
);
#59=(
BOUNDED_CURVE()
B_SPLINE_CURVE(2,(#23831,#23832,#23833,#23834,#23835,#23836,#23837,#23838,
#23839,#23840,#23841,#23842,#23843,#23844,#23845,#23846,#23847),
 .UNSPECIFIED.,.F.,.F.)
B_SPLINE_CURVE_WITH_KNOTS((3,2,2,2,2,2,2,2,3),(0.178571428571429,0.1875,
0.196428571428571,0.205357142857143,0.214285714285714,0.223214285714286,
0.232142857142857,0.241071428571429,0.25),.UNSPECIFIED.)
CURVE()
GEOMETRIC_REPRESENTATION_ITEM()
RATIONAL_B_SPLINE_CURVE((1.,0.923879532511287,1.,0.923879532511287,1.,0.923879532511287,
1.,0.923879532511287,1.,0.923879532511287,1.,0.923879532511287,1.,0.923879532511287,
1.,0.923879532511287,1.))
REPRESENTATION_ITEM('')
);
#60=(
BOUNDED_CURVE()
B_SPLINE_CURVE(2,(#23852,#23853,#23854,#23855,#23856,#23857,#23858,#23859,
#23860,#23861,#23862,#23863,#23864,#23865,#23866,#23867,#23868),
 .UNSPECIFIED.,.F.,.F.)
B_SPLINE_CURVE_WITH_KNOTS((3,2,2,2,2,2,2,2,3),(0.107142857142857,0.116071428571429,
0.125,0.133928571428571,0.142857142857143,0.151785714285714,0.160714285714286,
0.169642857142857,0.178571428571429),.UNSPECIFIED.)
CURVE()
GEOMETRIC_REPRESENTATION_ITEM()
RATIONAL_B_SPLINE_CURVE((1.,0.923879532511287,1.,0.923879532511287,1.,0.923879532511287,
1.,0.923879532511287,1.,0.923879532511287,1.,0.923879532511287,1.,0.923879532511287,
1.,0.923879532511287,1.))
REPRESENTATION_ITEM('')
);
#61=(
BOUNDED_CURVE()
B_SPLINE_CURVE(2,(#23869,#23870,#23871,#23872,#23873,#23874,#23875,#23876,
#23877,#23878,#23879,#23880,#23881,#23882,#23883,#23884,#23885),
 .UNSPECIFIED.,.F.,.F.)
B_SPLINE_CURVE_WITH_KNOTS((3,2,2,2,2,2,2,2,3),(0.107142857142857,0.116071428571429,
0.125,0.133928571428571,0.142857142857143,0.151785714285714,0.160714285714286,
0.169642857142857,0.178571428571429),.UNSPECIFIED.)
CURVE()
GEOMETRIC_REPRESENTATION_ITEM()
RATIONAL_B_SPLINE_CURVE((1.,0.923879532511287,1.,0.923879532511287,1.,0.923879532511287,
1.,0.923879532511287,1.,0.923879532511287,1.,0.923879532511287,1.,0.923879532511287,
1.,0.923879532511287,1.))
REPRESENTATION_ITEM('')
);
#62=(
BOUNDED_CURVE()
B_SPLINE_CURVE(2,(#25481,#25482,#25483,#25484,#25485,#25486,#25487),
 .UNSPECIFIED.,.F.,.F.)
B_SPLINE_CURVE_WITH_KNOTS((3,2,2,3),(0.0819392927096003,0.0892857142857143,
0.0982142857142857,0.107142857142857),.UNSPECIFIED.)
CURVE()
GEOMETRIC_REPRESENTATION_ITEM()
RATIONAL_B_SPLINE_CURVE((0.977803170316603,0.937368138988787,1.,0.923879532511287,
1.,0.923879532511287,1.))
REPRESENTATION_ITEM('')
);
#63=(
BOUNDED_CURVE()
B_SPLINE_CURVE(2,(#25489,#25490,#25491,#25492,#25493,#25494,#25495,#25496,
#25497,#25498,#25499),.UNSPECIFIED.,.F.,.F.)
B_SPLINE_CURVE_WITH_KNOTS((3,2,2,2,2,3),(0.0640821498524563,0.0714285714285714,
0.0803571428571429,0.0892857142857143,0.0982142857142857,0.107142857142857),
 .UNSPECIFIED.)
CURVE()
GEOMETRIC_REPRESENTATION_ITEM()
RATIONAL_B_SPLINE_CURVE((0.977803170316615,0.937368138988778,1.,0.923879532511287,
1.,0.923879532511287,1.,0.923879532511287,1.,0.923879532511287,1.))
REPRESENTATION_ITEM('')
);
#64=(
BOUNDED_CURVE()
B_SPLINE_CURVE(2,(#25959,#25960,#25961,#25962,#25963,#25964,#25965,#25966,
#25967,#25968,#25969,#25970,#25971,#25972,#25973),.UNSPECIFIED.,.F.,.F.)
B_SPLINE_CURVE_WITH_KNOTS((3,2,2,2,2,2,2,3),(0.168750000131362,0.175,0.1875,
0.2,0.2125,0.225,0.2375,0.25),.UNSPECIFIED.)
CURVE()
GEOMETRIC_REPRESENTATION_ITEM()
RATIONAL_B_SPLINE_CURVE((0.961939766255643,0.961939767055589,1.,0.923879532511287,
1.,0.923879532511287,1.,0.923879532511287,1.,0.923879532511287,1.,0.923879532511287,
1.,0.923879532511287,1.))
REPRESENTATION_ITEM('')
);
#65=(
BOUNDED_CURVE()
B_SPLINE_CURVE(2,(#25976,#25977,#25978,#25979,#25980,#25981,#25982,#25983,
#25984,#25985,#25986,#25987,#25988,#25989,#25990,#25991,#25992),
 .UNSPECIFIED.,.F.,.F.)
B_SPLINE_CURVE_WITH_KNOTS((3,2,2,2,2,2,2,2,3),(0.156250000131362,0.1625,
0.175,0.1875,0.2,0.2125,0.225,0.2375,0.25),.UNSPECIFIED.)
CURVE()
GEOMETRIC_REPRESENTATION_ITEM()
RATIONAL_B_SPLINE_CURVE((0.961939766255643,0.961939767055589,1.,0.923879532511287,
1.,0.923879532511287,1.,0.923879532511287,1.,0.923879532511287,1.,0.923879532511287,
1.,0.923879532511287,1.,0.923879532511287,1.))
REPRESENTATION_ITEM('')
);
#66=(
BOUNDED_CURVE()
B_SPLINE_CURVE(2,(#25997,#25998,#25999,#26000,#26001,#26002,#26003,#26004,
#26005,#26006,#26007,#26008,#26009,#26010,#26011,#26012,#26013),
 .UNSPECIFIED.,.F.,.F.)
B_SPLINE_CURVE_WITH_KNOTS((3,2,2,2,2,2,2,2,3),(0.25,0.2625,0.275,0.2875,
0.3,0.3125,0.325,0.3375,0.35),.UNSPECIFIED.)
CURVE()
GEOMETRIC_REPRESENTATION_ITEM()
RATIONAL_B_SPLINE_CURVE((1.,0.923879532511287,1.,0.923879532511287,1.,0.923879532511287,
1.,0.923879532511287,1.,0.923879532511287,1.,0.923879532511287,1.,0.923879532511287,
1.,0.923879532511287,1.))
REPRESENTATION_ITEM('')
);
#67=(
BOUNDED_CURVE()
B_SPLINE_CURVE(2,(#26014,#26015,#26016,#26017,#26018,#26019,#26020,#26021,
#26022,#26023,#26024,#26025,#26026,#26027,#26028,#26029,#26030),
 .UNSPECIFIED.,.F.,.F.)
B_SPLINE_CURVE_WITH_KNOTS((3,2,2,2,2,2,2,2,3),(0.25,0.2625,0.275,0.2875,
0.3,0.3125,0.325,0.3375,0.35),.UNSPECIFIED.)
CURVE()
GEOMETRIC_REPRESENTATION_ITEM()
RATIONAL_B_SPLINE_CURVE((1.,0.923879532511287,1.,0.923879532511287,1.,0.923879532511287,
1.,0.923879532511287,1.,0.923879532511287,1.,0.923879532511287,1.,0.923879532511287,
1.,0.923879532511287,1.))
REPRESENTATION_ITEM('')
);
#68=(
BOUNDED_CURVE()
B_SPLINE_CURVE(2,(#26035,#26036,#26037,#26038,#26039,#26040,#26041,#26042,
#26043,#26044,#26045,#26046,#26047,#26048,#26049,#26050,#26051),
 .UNSPECIFIED.,.F.,.F.)
B_SPLINE_CURVE_WITH_KNOTS((3,2,2,2,2,2,2,2,3),(0.35,0.3625,0.375,0.3875,
0.4,0.4125,0.425,0.4375,0.45),.UNSPECIFIED.)
CURVE()
GEOMETRIC_REPRESENTATION_ITEM()
RATIONAL_B_SPLINE_CURVE((1.,0.923879532511287,1.,0.923879532511287,1.,0.923879532511287,
1.,0.923879532511287,1.,0.923879532511287,1.,0.923879532511287,1.,0.923879532511287,
1.,0.923879532511287,1.))
REPRESENTATION_ITEM('')
);
#69=(
BOUNDED_CURVE()
B_SPLINE_CURVE(2,(#26052,#26053,#26054,#26055,#26056,#26057,#26058,#26059,
#26060,#26061,#26062,#26063,#26064,#26065,#26066,#26067,#26068),
 .UNSPECIFIED.,.F.,.F.)
B_SPLINE_CURVE_WITH_KNOTS((3,2,2,2,2,2,2,2,3),(0.35,0.3625,0.375,0.3875,
0.4,0.4125,0.425,0.4375,0.45),.UNSPECIFIED.)
CURVE()
GEOMETRIC_REPRESENTATION_ITEM()
RATIONAL_B_SPLINE_CURVE((1.,0.923879532511287,1.,0.923879532511287,1.,0.923879532511287,
1.,0.923879532511287,1.,0.923879532511287,1.,0.923879532511287,1.,0.923879532511287,
1.,0.923879532511287,1.))
REPRESENTATION_ITEM('')
);
#70=(
BOUNDED_CURVE()
B_SPLINE_CURVE(2,(#26073,#26074,#26075,#26076,#26077,#26078,#26079,#26080,
#26081,#26082,#26083,#26084,#26085,#26086,#26087,#26088,#26089),
 .UNSPECIFIED.,.F.,.F.)
B_SPLINE_CURVE_WITH_KNOTS((3,2,2,2,2,2,2,2,3),(0.45,0.4625,0.475,0.4875,
0.5,0.5125,0.525,0.5375,0.55),.UNSPECIFIED.)
CURVE()
GEOMETRIC_REPRESENTATION_ITEM()
RATIONAL_B_SPLINE_CURVE((1.,0.923879532511287,1.,0.923879532511287,1.,0.923879532511287,
1.,0.923879532511287,1.,0.923879532511287,1.,0.923879532511287,1.,0.923879532511287,
1.,0.923879532511287,1.))
REPRESENTATION_ITEM('')
);
#71=(
BOUNDED_CURVE()
B_SPLINE_CURVE(2,(#26090,#26091,#26092,#26093,#26094,#26095,#26096,#26097,
#26098,#26099,#26100,#26101,#26102,#26103,#26104,#26105,#26106),
 .UNSPECIFIED.,.F.,.F.)
B_SPLINE_CURVE_WITH_KNOTS((3,2,2,2,2,2,2,2,3),(0.45,0.4625,0.475,0.4875,
0.5,0.5125,0.525,0.5375,0.55),.UNSPECIFIED.)
CURVE()
GEOMETRIC_REPRESENTATION_ITEM()
RATIONAL_B_SPLINE_CURVE((1.,0.923879532511287,1.,0.923879532511287,1.,0.923879532511287,
1.,0.923879532511287,1.,0.923879532511287,1.,0.923879532511287,1.,0.923879532511287,
1.,0.923879532511287,1.))
REPRESENTATION_ITEM('')
);
#72=(
BOUNDED_CURVE()
B_SPLINE_CURVE(2,(#26111,#26112,#26113,#26114,#26115,#26116,#26117,#26118,
#26119,#26120,#26121,#26122,#26123,#26124,#26125,#26126,#26127),
 .UNSPECIFIED.,.F.,.F.)
B_SPLINE_CURVE_WITH_KNOTS((3,2,2,2,2,2,2,2,3),(0.55,0.5625,0.575,0.5875,
0.6,0.6125,0.625,0.6375,0.65),.UNSPECIFIED.)
CURVE()
GEOMETRIC_REPRESENTATION_ITEM()
RATIONAL_B_SPLINE_CURVE((1.,0.923879532511287,1.,0.923879532511287,1.,0.923879532511287,
1.,0.923879532511287,1.,0.923879532511287,1.,0.923879532511287,1.,0.923879532511287,
1.,0.923879532511287,1.))
REPRESENTATION_ITEM('')
);
#73=(
BOUNDED_CURVE()
B_SPLINE_CURVE(2,(#26128,#26129,#26130,#26131,#26132,#26133,#26134,#26135,
#26136,#26137,#26138,#26139,#26140,#26141,#26142,#26143,#26144),
 .UNSPECIFIED.,.F.,.F.)
B_SPLINE_CURVE_WITH_KNOTS((3,2,2,2,2,2,2,2,3),(0.55,0.5625,0.575,0.5875,
0.6,0.6125,0.625,0.6375,0.65),.UNSPECIFIED.)
CURVE()
GEOMETRIC_REPRESENTATION_ITEM()
RATIONAL_B_SPLINE_CURVE((1.,0.923879532511287,1.,0.923879532511287,1.,0.923879532511287,
1.,0.923879532511287,1.,0.923879532511287,1.,0.923879532511287,1.,0.923879532511287,
1.,0.923879532511287,1.))
REPRESENTATION_ITEM('')
);
#74=(
BOUNDED_CURVE()
B_SPLINE_CURVE(2,(#26149,#26150,#26151,#26152,#26153,#26154,#26155,#26156,
#26157,#26158,#26159,#26160,#26161,#26162,#26163,#26164,#26165),
 .UNSPECIFIED.,.F.,.F.)
B_SPLINE_CURVE_WITH_KNOTS((3,2,2,2,2,2,2,2,3),(0.65,0.6625,0.675,0.6875,
0.7,0.7125,0.725,0.7375,0.75),.UNSPECIFIED.)
CURVE()
GEOMETRIC_REPRESENTATION_ITEM()
RATIONAL_B_SPLINE_CURVE((1.,0.923879532511287,1.,0.923879532511287,1.,0.923879532511287,
1.,0.923879532511287,1.,0.923879532511287,1.,0.923879532511287,1.,0.923879532511287,
1.,0.923879532511287,1.))
REPRESENTATION_ITEM('')
);
#75=(
BOUNDED_CURVE()
B_SPLINE_CURVE(2,(#26166,#26167,#26168,#26169,#26170,#26171,#26172,#26173,
#26174,#26175,#26176,#26177,#26178,#26179,#26180,#26181,#26182),
 .UNSPECIFIED.,.F.,.F.)
B_SPLINE_CURVE_WITH_KNOTS((3,2,2,2,2,2,2,2,3),(0.65,0.6625,0.675,0.6875,
0.7,0.7125,0.725,0.7375,0.75),.UNSPECIFIED.)
CURVE()
GEOMETRIC_REPRESENTATION_ITEM()
RATIONAL_B_SPLINE_CURVE((1.,0.923879532511287,1.,0.923879532511287,1.,0.923879532511287,
1.,0.923879532511287,1.,0.923879532511287,1.,0.923879532511287,1.,0.923879532511287,
1.,0.923879532511287,1.))
REPRESENTATION_ITEM('')
);
#76=(
BOUNDED_CURVE()
B_SPLINE_CURVE(2,(#26187,#26188,#26189,#26190,#26191,#26192,#26193,#26194,
#26195,#26196,#26197,#26198,#26199,#26200,#26201,#26202,#26203),
 .UNSPECIFIED.,.F.,.F.)
B_SPLINE_CURVE_WITH_KNOTS((3,2,2,2,2,2,2,2,3),(0.75,0.7625,0.775,0.7875,
0.8,0.8125,0.825,0.8375,0.85),.UNSPECIFIED.)
CURVE()
GEOMETRIC_REPRESENTATION_ITEM()
RATIONAL_B_SPLINE_CURVE((1.,0.923879532511287,1.,0.923879532511287,1.,0.923879532511287,
1.,0.923879532511287,1.,0.923879532511287,1.,0.923879532511287,1.,0.923879532511287,
1.,0.923879532511287,1.))
REPRESENTATION_ITEM('')
);
#77=(
BOUNDED_CURVE()
B_SPLINE_CURVE(2,(#26204,#26205,#26206,#26207,#26208,#26209,#26210,#26211,
#26212,#26213,#26214,#26215,#26216,#26217,#26218,#26219,#26220),
 .UNSPECIFIED.,.F.,.F.)
B_SPLINE_CURVE_WITH_KNOTS((3,2,2,2,2,2,2,2,3),(0.75,0.7625,0.775,0.7875,
0.8,0.8125,0.825,0.8375,0.85),.UNSPECIFIED.)
CURVE()
GEOMETRIC_REPRESENTATION_ITEM()
RATIONAL_B_SPLINE_CURVE((1.,0.923879532511287,1.,0.923879532511287,1.,0.923879532511287,
1.,0.923879532511287,1.,0.923879532511287,1.,0.923879532511287,1.,0.923879532511287,
1.,0.923879532511287,1.))
REPRESENTATION_ITEM('')
);
#78=(
BOUNDED_CURVE()
B_SPLINE_CURVE(2,(#26226,#26227,#26228,#26229,#26230,#26231,#26232,#26233,
#26234),.UNSPECIFIED.,.F.,.F.)
B_SPLINE_CURVE_WITH_KNOTS((3,2,2,2,3),(0.95,0.9625,0.975,0.9875,1.),
 .UNSPECIFIED.)
CURVE()
GEOMETRIC_REPRESENTATION_ITEM()
RATIONAL_B_SPLINE_CURVE((1.,0.923879532511287,1.,0.923879532511287,1.,0.923879532511287,
1.,0.923879532511287,1.))
REPRESENTATION_ITEM('')
);
#79=(
BOUNDED_CURVE()
B_SPLINE_CURVE(2,(#26237,#26238,#26239,#26240,#26241,#26242,#26243,#26244,
#26245),.UNSPECIFIED.,.F.,.F.)
B_SPLINE_CURVE_WITH_KNOTS((3,2,2,2,3),(0.95,0.9625,0.975,0.9875,1.),
 .UNSPECIFIED.)
CURVE()
GEOMETRIC_REPRESENTATION_ITEM()
RATIONAL_B_SPLINE_CURVE((1.,0.923879532511287,1.,0.923879532511287,1.,0.923879532511287,
1.,0.923879532511287,1.))
REPRESENTATION_ITEM('')
);
#80=(
BOUNDED_CURVE()
B_SPLINE_CURVE(2,(#27008,#27009,#27010,#27011,#27012,#27013,#27014,#27015,
#27016,#27017,#27018,#27019,#27020,#27021,#27022,#27023,#27024),
 .UNSPECIFIED.,.F.,.F.)
B_SPLINE_CURVE_WITH_KNOTS((3,2,2,2,2,2,2,2,3),(0.85,0.8625,0.875,0.8875,
0.9,0.9125,0.925,0.9375,0.95),.UNSPECIFIED.)
CURVE()
GEOMETRIC_REPRESENTATION_ITEM()
RATIONAL_B_SPLINE_CURVE((1.,0.923879532511287,1.,0.923879532511287,1.,0.923879532511287,
1.,0.923879532511287,1.,0.923879532511287,1.,0.923879532511287,1.,0.923879532511287,
1.,0.923879532511287,1.))
REPRESENTATION_ITEM('')
);
#81=(
BOUNDED_CURVE()
B_SPLINE_CURVE(2,(#27025,#27026,#27027,#27028,#27029,#27030,#27031,#27032,
#27033,#27034,#27035,#27036,#27037,#27038,#27039,#27040,#27041),
 .UNSPECIFIED.,.F.,.F.)
B_SPLINE_CURVE_WITH_KNOTS((3,2,2,2,2,2,2,2,3),(0.85,0.8625,0.875,0.8875,
0.9,0.9125,0.925,0.9375,0.95),.UNSPECIFIED.)
CURVE()
GEOMETRIC_REPRESENTATION_ITEM()
RATIONAL_B_SPLINE_CURVE((1.,0.923879532511287,1.,0.923879532511287,1.,0.923879532511287,
1.,0.923879532511287,1.,0.923879532511287,1.,0.923879532511287,1.,0.923879532511287,
1.,0.923879532511287,1.))
REPRESENTATION_ITEM('')
);
#82=ITEM_DEFINED_TRANSFORMATION($,$,#12653,#12782);
#83=ITEM_DEFINED_TRANSFORMATION($,$,#12749,#12783);
#84=ITEM_DEFINED_TRANSFORMATION($,$,#12785,#12965);
#85=ITEM_DEFINED_TRANSFORMATION($,$,#12859,#12966);
#86=ITEM_DEFINED_TRANSFORMATION($,$,#12944,#12967);
#87=ITEM_DEFINED_TRANSFORMATION($,$,#12994,#13361);
#88=ITEM_DEFINED_TRANSFORMATION($,$,#13164,#13362);
#89=ITEM_DEFINED_TRANSFORMATION($,$,#13186,#13363);
#90=ITEM_DEFINED_TRANSFORMATION($,$,#13208,#13364);
#91=ITEM_DEFINED_TRANSFORMATION($,$,#13212,#13365);
#92=ITEM_DEFINED_TRANSFORMATION($,$,#13263,#13366);
#93=ITEM_DEFINED_TRANSFORMATION($,$,#13302,#13367);
#94=ITEM_DEFINED_TRANSFORMATION($,$,#13369,#13452);
#95=ITEM_DEFINED_TRANSFORMATION($,$,#13422,#13453);
#96=ITEM_DEFINED_TRANSFORMATION($,$,#13434,#13454);
#97=ITEM_DEFINED_TRANSFORMATION($,$,#13456,#13512);
#98=ITEM_DEFINED_TRANSFORMATION($,$,#13467,#13513);
#99=ITEM_DEFINED_TRANSFORMATION($,$,#13467,#13514);
#100=ITEM_DEFINED_TRANSFORMATION($,$,#12299,#13719);
#101=ITEM_DEFINED_TRANSFORMATION($,$,#12652,#13720);
#102=ITEM_DEFINED_TRANSFORMATION($,$,#12784,#13721);
#103=ITEM_DEFINED_TRANSFORMATION($,$,#12968,#13722);
#104=ITEM_DEFINED_TRANSFORMATION($,$,#12968,#13723);
#105=ITEM_DEFINED_TRANSFORMATION($,$,#12993,#13724);
#106=ITEM_DEFINED_TRANSFORMATION($,$,#13368,#13725);
#107=ITEM_DEFINED_TRANSFORMATION($,$,#13455,#13726);
#108=ITEM_DEFINED_TRANSFORMATION($,$,#13515,#13727);
#109=ITEM_DEFINED_TRANSFORMATION($,$,#13515,#13728);
#110=ITEM_DEFINED_TRANSFORMATION($,$,#13693,#13729);
#111=ITEM_DEFINED_TRANSFORMATION($,$,#13693,#13730);
#112=ITEM_DEFINED_TRANSFORMATION($,$,#13708,#13731);
#113=(
REPRESENTATION_RELATIONSHIP($,$,#27902,#27901)
REPRESENTATION_RELATIONSHIP_WITH_TRANSFORMATION(#82)
SHAPE_REPRESENTATION_RELATIONSHIP()
);
#114=(
REPRESENTATION_RELATIONSHIP($,$,#27903,#27901)
REPRESENTATION_RELATIONSHIP_WITH_TRANSFORMATION(#83)
SHAPE_REPRESENTATION_RELATIONSHIP()
);
#115=(
REPRESENTATION_RELATIONSHIP($,$,#27905,#27904)
REPRESENTATION_RELATIONSHIP_WITH_TRANSFORMATION(#84)
SHAPE_REPRESENTATION_RELATIONSHIP()
);
#116=(
REPRESENTATION_RELATIONSHIP($,$,#27906,#27904)
REPRESENTATION_RELATIONSHIP_WITH_TRANSFORMATION(#85)
SHAPE_REPRESENTATION_RELATIONSHIP()
);
#117=(
REPRESENTATION_RELATIONSHIP($,$,#27907,#27904)
REPRESENTATION_RELATIONSHIP_WITH_TRANSFORMATION(#86)
SHAPE_REPRESENTATION_RELATIONSHIP()
);
#118=(
REPRESENTATION_RELATIONSHIP($,$,#27910,#27909)
REPRESENTATION_RELATIONSHIP_WITH_TRANSFORMATION(#87)
SHAPE_REPRESENTATION_RELATIONSHIP()
);
#119=(
REPRESENTATION_RELATIONSHIP($,$,#27911,#27909)
REPRESENTATION_RELATIONSHIP_WITH_TRANSFORMATION(#88)
SHAPE_REPRESENTATION_RELATIONSHIP()
);
#120=(
REPRESENTATION_RELATIONSHIP($,$,#27912,#27909)
REPRESENTATION_RELATIONSHIP_WITH_TRANSFORMATION(#89)
SHAPE_REPRESENTATION_RELATIONSHIP()
);
#121=(
REPRESENTATION_RELATIONSHIP($,$,#27913,#27909)
REPRESENTATION_RELATIONSHIP_WITH_TRANSFORMATION(#90)
SHAPE_REPRESENTATION_RELATIONSHIP()
);
#122=(
REPRESENTATION_RELATIONSHIP($,$,#27914,#27909)
REPRESENTATION_RELATIONSHIP_WITH_TRANSFORMATION(#91)
SHAPE_REPRESENTATION_RELATIONSHIP()
);
#123=(
REPRESENTATION_RELATIONSHIP($,$,#27915,#27909)
REPRESENTATION_RELATIONSHIP_WITH_TRANSFORMATION(#92)
SHAPE_REPRESENTATION_RELATIONSHIP()
);
#124=(
REPRESENTATION_RELATIONSHIP($,$,#27916,#27909)
REPRESENTATION_RELATIONSHIP_WITH_TRANSFORMATION(#93)
SHAPE_REPRESENTATION_RELATIONSHIP()
);
#125=(
REPRESENTATION_RELATIONSHIP($,$,#27918,#27917)
REPRESENTATION_RELATIONSHIP_WITH_TRANSFORMATION(#94)
SHAPE_REPRESENTATION_RELATIONSHIP()
);
#126=(
REPRESENTATION_RELATIONSHIP($,$,#27919,#27917)
REPRESENTATION_RELATIONSHIP_WITH_TRANSFORMATION(#95)
SHAPE_REPRESENTATION_RELATIONSHIP()
);
#127=(
REPRESENTATION_RELATIONSHIP($,$,#27920,#27917)
REPRESENTATION_RELATIONSHIP_WITH_TRANSFORMATION(#96)
SHAPE_REPRESENTATION_RELATIONSHIP()
);
#128=(
REPRESENTATION_RELATIONSHIP($,$,#27922,#27921)
REPRESENTATION_RELATIONSHIP_WITH_TRANSFORMATION(#97)
SHAPE_REPRESENTATION_RELATIONSHIP()
);
#129=(
REPRESENTATION_RELATIONSHIP($,$,#27923,#27921)
REPRESENTATION_RELATIONSHIP_WITH_TRANSFORMATION(#98)
SHAPE_REPRESENTATION_RELATIONSHIP()
);
#130=(
REPRESENTATION_RELATIONSHIP($,$,#27923,#27921)
REPRESENTATION_RELATIONSHIP_WITH_TRANSFORMATION(#99)
SHAPE_REPRESENTATION_RELATIONSHIP()
);
#131=(
REPRESENTATION_RELATIONSHIP($,$,#27900,#27899)
REPRESENTATION_RELATIONSHIP_WITH_TRANSFORMATION(#100)
SHAPE_REPRESENTATION_RELATIONSHIP()
);
#132=(
REPRESENTATION_RELATIONSHIP($,$,#27901,#27899)
REPRESENTATION_RELATIONSHIP_WITH_TRANSFORMATION(#101)
SHAPE_REPRESENTATION_RELATIONSHIP()
);
#133=(
REPRESENTATION_RELATIONSHIP($,$,#27904,#27899)
REPRESENTATION_RELATIONSHIP_WITH_TRANSFORMATION(#102)
SHAPE_REPRESENTATION_RELATIONSHIP()
);
#134=(
REPRESENTATION_RELATIONSHIP($,$,#27908,#27899)
REPRESENTATION_RELATIONSHIP_WITH_TRANSFORMATION(#103)
SHAPE_REPRESENTATION_RELATIONSHIP()
);
#135=(
REPRESENTATION_RELATIONSHIP($,$,#27908,#27899)
REPRESENTATION_RELATIONSHIP_WITH_TRANSFORMATION(#104)
SHAPE_REPRESENTATION_RELATIONSHIP()
);
#136=(
REPRESENTATION_RELATIONSHIP($,$,#27909,#27899)
REPRESENTATION_RELATIONSHIP_WITH_TRANSFORMATION(#105)
SHAPE_REPRESENTATION_RELATIONSHIP()
);
#137=(
REPRESENTATION_RELATIONSHIP($,$,#27917,#27899)
REPRESENTATION_RELATIONSHIP_WITH_TRANSFORMATION(#106)
SHAPE_REPRESENTATION_RELATIONSHIP()
);
#138=(
REPRESENTATION_RELATIONSHIP($,$,#27921,#27899)
REPRESENTATION_RELATIONSHIP_WITH_TRANSFORMATION(#107)
SHAPE_REPRESENTATION_RELATIONSHIP()
);
#139=(
REPRESENTATION_RELATIONSHIP($,$,#27924,#27899)
REPRESENTATION_RELATIONSHIP_WITH_TRANSFORMATION(#108)
SHAPE_REPRESENTATION_RELATIONSHIP()
);
#140=(
REPRESENTATION_RELATIONSHIP($,$,#27924,#27899)
REPRESENTATION_RELATIONSHIP_WITH_TRANSFORMATION(#109)
SHAPE_REPRESENTATION_RELATIONSHIP()
);
#141=(
REPRESENTATION_RELATIONSHIP($,$,#27925,#27899)
REPRESENTATION_RELATIONSHIP_WITH_TRANSFORMATION(#110)
SHAPE_REPRESENTATION_RELATIONSHIP()
);
#142=(
REPRESENTATION_RELATIONSHIP($,$,#27925,#27899)
REPRESENTATION_RELATIONSHIP_WITH_TRANSFORMATION(#111)
SHAPE_REPRESENTATION_RELATIONSHIP()
);
#143=(
REPRESENTATION_RELATIONSHIP($,$,#27926,#27899)
REPRESENTATION_RELATIONSHIP_WITH_TRANSFORMATION(#112)
SHAPE_REPRESENTATION_RELATIONSHIP()
);
#144=CONTEXT_DEPENDENT_SHAPE_REPRESENTATION(#113,#27845);
#145=CONTEXT_DEPENDENT_SHAPE_REPRESENTATION(#114,#27846);
#146=CONTEXT_DEPENDENT_SHAPE_REPRESENTATION(#115,#27851);
#147=CONTEXT_DEPENDENT_SHAPE_REPRESENTATION(#116,#27852);
#148=CONTEXT_DEPENDENT_SHAPE_REPRESENTATION(#117,#27853);
#149=CONTEXT_DEPENDENT_SHAPE_REPRESENTATION(#118,#27863);
#150=CONTEXT_DEPENDENT_SHAPE_REPRESENTATION(#119,#27864);
#151=CONTEXT_DEPENDENT_SHAPE_REPRESENTATION(#120,#27865);
#152=CONTEXT_DEPENDENT_SHAPE_REPRESENTATION(#121,#27866);
#153=CONTEXT_DEPENDENT_SHAPE_REPRESENTATION(#122,#27867);
#154=CONTEXT_DEPENDENT_SHAPE_REPRESENTATION(#123,#27868);
#155=CONTEXT_DEPENDENT_SHAPE_REPRESENTATION(#124,#27869);
#156=CONTEXT_DEPENDENT_SHAPE_REPRESENTATION(#125,#27874);
#157=CONTEXT_DEPENDENT_SHAPE_REPRESENTATION(#126,#27875);
#158=CONTEXT_DEPENDENT_SHAPE_REPRESENTATION(#127,#27876);
#159=CONTEXT_DEPENDENT_SHAPE_REPRESENTATION(#128,#27880);
#160=CONTEXT_DEPENDENT_SHAPE_REPRESENTATION(#129,#27881);
#161=CONTEXT_DEPENDENT_SHAPE_REPRESENTATION(#130,#27882);
#162=CONTEXT_DEPENDENT_SHAPE_REPRESENTATION(#131,#27886);
#163=CONTEXT_DEPENDENT_SHAPE_REPRESENTATION(#132,#27887);
#164=CONTEXT_DEPENDENT_SHAPE_REPRESENTATION(#133,#27888);
#165=CONTEXT_DEPENDENT_SHAPE_REPRESENTATION(#134,#27889);
#166=CONTEXT_DEPENDENT_SHAPE_REPRESENTATION(#135,#27890);
#167=CONTEXT_DEPENDENT_SHAPE_REPRESENTATION(#136,#27891);
#168=CONTEXT_DEPENDENT_SHAPE_REPRESENTATION(#137,#27892);
#169=CONTEXT_DEPENDENT_SHAPE_REPRESENTATION(#138,#27893);
#170=CONTEXT_DEPENDENT_SHAPE_REPRESENTATION(#139,#27894);
#171=CONTEXT_DEPENDENT_SHAPE_REPRESENTATION(#140,#27895);
#172=CONTEXT_DEPENDENT_SHAPE_REPRESENTATION(#141,#27896);
#173=CONTEXT_DEPENDENT_SHAPE_REPRESENTATION(#142,#27897);
#174=CONTEXT_DEPENDENT_SHAPE_REPRESENTATION(#143,#27898);
#175=NEXT_ASSEMBLY_USAGE_OCCURRENCE('Lifting Arm:1','Lifting Arm:1',
'Lifting Arm:1',#27930,#27931,'Lifting Arm:1');
#176=NEXT_ASSEMBLY_USAGE_OCCURRENCE('Arm Rollers:1','Arm Rollers:1',
'Arm Rollers:1',#27930,#27932,'Arm Rollers:1');
#177=NEXT_ASSEMBLY_USAGE_OCCURRENCE('Lifting Saddle:1',
'Lifting Saddle:1','Lifting Saddle:1',#27933,#27934,'Lifting Saddle:1');
#178=NEXT_ASSEMBLY_USAGE_OCCURRENCE('Saddle Holder:1','Saddle Holder:1',
'Saddle Holder:1',#27933,#27935,'Saddle Holder:1');
#179=NEXT_ASSEMBLY_USAGE_OCCURRENCE('Saddle Pins:1','Saddle Pins:1',
'Saddle Pins:1',#27933,#27936,'Saddle Pins:1');
#180=NEXT_ASSEMBLY_USAGE_OCCURRENCE('Pump Body:1','Pump Body:1',
'Pump Body:1',#27938,#27939,'Pump Body:1');
#181=NEXT_ASSEMBLY_USAGE_OCCURRENCE('Hydraulic Ram:1','Hydraulic Ram:1',
'Hydraulic Ram:1',#27938,#27940,'Hydraulic Ram:1');
#182=NEXT_ASSEMBLY_USAGE_OCCURRENCE('Release Valve Screw:1',
'Release Valve Screw:1','Release Valve Screw:1',#27938,#27941,
'Release Valve Screw:1');
#183=NEXT_ASSEMBLY_USAGE_OCCURRENCE('Valve Ball:1','Valve Ball:1',
'Valve Ball:1',#27938,#27942,'Valve Ball:1');
#184=NEXT_ASSEMBLY_USAGE_OCCURRENCE('Valve Fitting:1','Valve Fitting:1',
'Valve Fitting:1',#27938,#27943,'Valve Fitting:1');
#185=NEXT_ASSEMBLY_USAGE_OCCURRENCE('Pump Pins:1','Pump Pins:1',
'Pump Pins:1',#27938,#27944,'Pump Pins:1');
#186=NEXT_ASSEMBLY_USAGE_OCCURRENCE('Retaining Clips:1',
'Retaining Clips:1','Retaining Clips:1',#27938,#27945,
'Retaining Clips:1');
#187=NEXT_ASSEMBLY_USAGE_OCCURRENCE('Handle Socket:1','Handle Socket:1',
'Handle Socket:1',#27946,#27947,'Handle Socket:1');
#188=NEXT_ASSEMBLY_USAGE_OCCURRENCE('Handle Tube:1','Handle Tube:1',
'Handle Tube:1',#27946,#27948,'Handle Tube:1');
#189=NEXT_ASSEMBLY_USAGE_OCCURRENCE('Handle Grip:1','Handle Grip:1',
'Handle Grip:1',#27946,#27949,'Handle Grip:1');
#190=NEXT_ASSEMBLY_USAGE_OCCURRENCE('Front Axle:1','Front Axle:1',
'Front Axle:1',#27950,#27951,'Front Axle:1');
#191=NEXT_ASSEMBLY_USAGE_OCCURRENCE('Front Wheel:1','Front Wheel:1',
'Front Wheel:1',#27950,#27952,'Front Wheel:1');
#192=NEXT_ASSEMBLY_USAGE_OCCURRENCE('Front Wheel:2','Front Wheel:2',
'Front Wheel:2',#27950,#27952,'Front Wheel:2');
#193=NEXT_ASSEMBLY_USAGE_OCCURRENCE('Main Frame:1','Main Frame:1',
'Main Frame:1',#27928,#27929,'Main Frame:1');
#194=NEXT_ASSEMBLY_USAGE_OCCURRENCE('Lifting Arm Assembly:1',
'Lifting Arm Assembly:1','Lifting Arm Assembly:1',#27928,#27930,
'Lifting Arm Assembly:1');
#195=NEXT_ASSEMBLY_USAGE_OCCURRENCE('Saddle Assembly:1',
'Saddle Assembly:1','Saddle Assembly:1',#27928,#27933,
'Saddle Assembly:1');
#196=NEXT_ASSEMBLY_USAGE_OCCURRENCE('Saddle Link:1','Saddle Link:1',
'Saddle Link:1',#27928,#27937,'Saddle Link:1');
#197=NEXT_ASSEMBLY_USAGE_OCCURRENCE('Saddle Link:2','Saddle Link:2',
'Saddle Link:2',#27928,#27937,'Saddle Link:2');
#198=NEXT_ASSEMBLY_USAGE_OCCURRENCE('Hydraulic Pump Unit:1',
'Hydraulic Pump Unit:1','Hydraulic Pump Unit:1',#27928,#27938,
'Hydraulic Pump Unit:1');
#199=NEXT_ASSEMBLY_USAGE_OCCURRENCE('Handle Assembly:1',
'Handle Assembly:1','Handle Assembly:1',#27928,#27946,
'Handle Assembly:1');
#200=NEXT_ASSEMBLY_USAGE_OCCURRENCE('Front Wheel Assembly:1',
'Front Wheel Assembly:1','Front Wheel Assembly:1',#27928,#27950,
'Front Wheel Assembly:1');
#201=NEXT_ASSEMBLY_USAGE_OCCURRENCE('Rear Caster Wheel:1',
'Rear Caster Wheel:1','Rear Caster Wheel:1',#27928,#27953,
'Rear Caster Wheel:1');
#202=NEXT_ASSEMBLY_USAGE_OCCURRENCE('Rear Caster Wheel:2',
'Rear Caster Wheel:2','Rear Caster Wheel:2',#27928,#27953,
'Rear Caster Wheel:2');
#203=NEXT_ASSEMBLY_USAGE_OCCURRENCE('Pivot Pin Cap:1','Pivot Pin Cap:1',
'Pivot Pin Cap:1',#27928,#27954,'Pivot Pin Cap:1');
#204=NEXT_ASSEMBLY_USAGE_OCCURRENCE('Pivot Pin Cap:2','Pivot Pin Cap:2',
'Pivot Pin Cap:2',#27928,#27954,'Pivot Pin Cap:2');
#205=NEXT_ASSEMBLY_USAGE_OCCURRENCE('Handle Pivot Pin:1',
'Handle Pivot Pin:1','Handle Pivot Pin:1',#27928,#27955,
'Handle Pivot Pin:1');
#206=SHAPE_REPRESENTATION_RELATIONSHIP('SRR','None',#27900,#228);
#207=SHAPE_REPRESENTATION_RELATIONSHIP('SRR','None',#27902,#229);
#208=SHAPE_REPRESENTATION_RELATIONSHIP('SRR','None',#27903,#230);
#209=SHAPE_REPRESENTATION_RELATIONSHIP('SRR','None',#27905,#231);
#210=SHAPE_REPRESENTATION_RELATIONSHIP('SRR','None',#27906,#232);
#211=SHAPE_REPRESENTATION_RELATIONSHIP('SRR','None',#27907,#233);
#212=SHAPE_REPRESENTATION_RELATIONSHIP('SRR','None',#27908,#234);
#213=SHAPE_REPRESENTATION_RELATIONSHIP('SRR','None',#27910,#235);
#214=SHAPE_REPRESENTATION_RELATIONSHIP('SRR','None',#27911,#236);
#215=SHAPE_REPRESENTATION_RELATIONSHIP('SRR','None',#27912,#237);
#216=SHAPE_REPRESENTATION_RELATIONSHIP('SRR','None',#27913,#238);
#217=SHAPE_REPRESENTATION_RELATIONSHIP('SRR','None',#27914,#239);
#218=SHAPE_REPRESENTATION_RELATIONSHIP('SRR','None',#27915,#240);
#219=SHAPE_REPRESENTATION_RELATIONSHIP('SRR','None',#27916,#241);
#220=SHAPE_REPRESENTATION_RELATIONSHIP('SRR','None',#27918,#242);
#221=SHAPE_REPRESENTATION_RELATIONSHIP('SRR','None',#27919,#243);
#222=SHAPE_REPRESENTATION_RELATIONSHIP('SRR','None',#27920,#244);
#223=SHAPE_REPRESENTATION_RELATIONSHIP('SRR','None',#27922,#245);
#224=SHAPE_REPRESENTATION_RELATIONSHIP('SRR','None',#27923,#246);
#225=SHAPE_REPRESENTATION_RELATIONSHIP('SRR','None',#27924,#247);
#226=SHAPE_REPRESENTATION_RELATIONSHIP('SRR','None',#27925,#248);
#227=SHAPE_REPRESENTATION_RELATIONSHIP('SRR','None',#27926,#249);
#228=ADVANCED_BREP_SHAPE_REPRESENTATION('',(#279),#27780);
#229=ADVANCED_BREP_SHAPE_REPRESENTATION('',(#280),#27782);
#230=ADVANCED_BREP_SHAPE_REPRESENTATION('',(#281,#282),#27783);
#231=ADVANCED_BREP_SHAPE_REPRESENTATION('',(#283),#27785);
#232=ADVANCED_BREP_SHAPE_REPRESENTATION('',(#284),#27786);
#233=ADVANCED_BREP_SHAPE_REPRESENTATION('',(#285,#286),#27787);
#234=ADVANCED_BREP_SHAPE_REPRESENTATION('',(#287),#27788);
#235=ADVANCED_BREP_SHAPE_REPRESENTATION('',(#288),#27790);
#236=ADVANCED_BREP_SHAPE_REPRESENTATION('',(#289),#27791);
#237=ADVANCED_BREP_SHAPE_REPRESENTATION('',(#290),#27792);
#238=ADVANCED_BREP_SHAPE_REPRESENTATION('',(#291),#27793);
#239=ADVANCED_BREP_SHAPE_REPRESENTATION('',(#292),#27794);
#240=ADVANCED_BREP_SHAPE_REPRESENTATION('',(#293,#294),#27795);
#241=ADVANCED_BREP_SHAPE_REPRESENTATION('',(#295,#296),#27796);
#242=ADVANCED_BREP_SHAPE_REPRESENTATION('',(#297),#27798);
#243=ADVANCED_BREP_SHAPE_REPRESENTATION('',(#298),#27799);
#244=ADVANCED_BREP_SHAPE_REPRESENTATION('',(#299),#27800);
#245=ADVANCED_BREP_SHAPE_REPRESENTATION('',(#300),#27802);
#246=ADVANCED_BREP_SHAPE_REPRESENTATION('',(#301),#27803);
#247=ADVANCED_BREP_SHAPE_REPRESENTATION('',(#302,#303,#304,#305),#27804);
#248=ADVANCED_BREP_SHAPE_REPRESENTATION('',(#306),#27805);
#249=ADVANCED_BREP_SHAPE_REPRESENTATION('',(#307),#27806);
#250=STYLED_ITEM('',(#28056),#279);
#251=STYLED_ITEM('',(#28070),#280);
#252=STYLED_ITEM('',(#28063),#281);
#253=STYLED_ITEM('',(#28063),#282);
#254=STYLED_ITEM('',(#28070),#283);
#255=STYLED_ITEM('',(#28091),#284);
#256=STYLED_ITEM('',(#28063),#285);
#257=STYLED_ITEM('',(#28063),#286);
#258=STYLED_ITEM('',(#28091),#287);
#259=STYLED_ITEM('',(#28056),#288);
#260=STYLED_ITEM('',(#28070),#289);
#261=STYLED_ITEM('',(#28084),#290);
#262=STYLED_ITEM('',(#28063),#291);
#263=STYLED_ITEM('',(#28070),#292);
#264=STYLED_ITEM('',(#28063),#293);
#265=STYLED_ITEM('',(#28063),#294);
#266=STYLED_ITEM('',(#28070),#295);
#267=STYLED_ITEM('',(#28070),#296);
#268=STYLED_ITEM('',(#28070),#297);
#269=STYLED_ITEM('',(#28063),#298);
#270=STYLED_ITEM('',(#28084),#299);
#271=STYLED_ITEM('',(#28077),#300);
#272=STYLED_ITEM('',(#28070),#301);
#273=STYLED_ITEM('',(#28091),#302);
#274=STYLED_ITEM('',(#28091),#303);
#275=STYLED_ITEM('',(#28091),#304);
#276=STYLED_ITEM('',(#28091),#305);
#277=STYLED_ITEM('',(#28077),#306);
#278=STYLED_ITEM('',(#28077),#307);
#279=MANIFOLD_SOLID_BREP('Body1',#12026);
#280=MANIFOLD_SOLID_BREP('Body1',#12027);
#281=MANIFOLD_SOLID_BREP('Body1',#12028);
#282=MANIFOLD_SOLID_BREP('Body2',#12029);
#283=MANIFOLD_SOLID_BREP('Body1',#12030);
#284=MANIFOLD_SOLID_BREP('Body1',#12031);
#285=MANIFOLD_SOLID_BREP('Body1',#12032);
#286=MANIFOLD_SOLID_BREP('Body2',#12033);
#287=MANIFOLD_SOLID_BREP('Body1',#12034);
#288=MANIFOLD_SOLID_BREP('Body1',#12035);
#289=MANIFOLD_SOLID_BREP('Body1',#12036);
#290=MANIFOLD_SOLID_BREP('Body1',#12037);
#291=MANIFOLD_SOLID_BREP('Body1',#12038);
#292=MANIFOLD_SOLID_BREP('Body1',#12039);
#293=MANIFOLD_SOLID_BREP('Body1',#12040);
#294=MANIFOLD_SOLID_BREP('Body2',#12041);
#295=MANIFOLD_SOLID_BREP('Body1',#12042);
#296=MANIFOLD_SOLID_BREP('Body2',#12043);
#297=MANIFOLD_SOLID_BREP('Body1',#12044);
#298=MANIFOLD_SOLID_BREP('Body1',#12045);
#299=MANIFOLD_SOLID_BREP('Body1',#12046);
#300=MANIFOLD_SOLID_BREP('Body1',#12047);
#301=MANIFOLD_SOLID_BREP('Body1',#12048);
#302=MANIFOLD_SOLID_BREP('Body1',#12049);
#303=MANIFOLD_SOLID_BREP('Body2',#12050);
#304=MANIFOLD_SOLID_BREP('Body3',#12051);
#305=MANIFOLD_SOLID_BREP('Body4',#12052);
#306=MANIFOLD_SOLID_BREP('Body1',#12053);
#307=MANIFOLD_SOLID_BREP('Body1',#12054);
#308=(
BOUNDED_SURFACE()
B_SPLINE_SURFACE(3,2,((#18358,#18359,#18360),(#18361,#18362,#18363),(#18364,
#18365,#18366),(#18367,#18368,#18369),(#18370,#18371,#18372),(#18373,#18374,
#18375),(#18376,#18377,#18378),(#18379,#18380,#18381),(#18382,#18383,#18384),
(#18385,#18386,#18387),(#18388,#18389,#18390),(#18391,#18392,#18393)),
 .UNSPECIFIED.,.F.,.F.,.F.)
B_SPLINE_SURFACE_WITH_KNOTS((4,2,2,2,2,4),(3,3),(0.00614272984621533,0.00826669470830694,
0.0093243666888766,0.0103820386694462,0.0124973826305856,0.0146213474926772),
(-5.56138348356354E-6,1.00000862090095),.UNSPECIFIED.)
GEOMETRIC_REPRESENTATION_ITEM()
RATIONAL_B_SPLINE_SURFACE(((1.00000326161464,0.706759768309428,1.00000505596187),
(1.00000294808663,0.734947962870916,1.0000045699493),(1.00000271960407,
0.755490020803058,1.00000421576918),(1.00000249159586,0.775989432119934,
1.00000386232436),(1.00000243486445,0.781089952812372,1.00000377438268),
(1.00000236001445,0.787819451076599,1.00000365835465),(1.00000234158956,
0.789475967918314,1.00000362979347),(1.00000234175209,0.789461355655222,
1.00000363004541),(1.00000241511518,0.782865540172825,1.00000374376852),
(1.00000271619428,0.755796583331183,1.00000421048352),(1.00000294648698,
0.73509178111339,1.00000456746963),(1.00000326163437,0.706757994665561,
1.00000505599245)))
REPRESENTATION_ITEM('')
SURFACE()
);
#309=(
BOUNDED_SURFACE()
B_SPLINE_SURFACE(3,2,((#18394,#18395,#18396),(#18397,#18398,#18399),(#18400,
#18401,#18402),(#18403,#18404,#18405),(#18406,#18407,#18408),(#18409,#18410,
#18411),(#18412,#18413,#18414),(#18415,#18416,#18417),(#18418,#18419,#18420),
(#18421,#18422,#18423),(#18424,#18425,#18426),(#18427,#18428,#18429)),
 .UNSPECIFIED.,.F.,.F.,.F.)
B_SPLINE_SURFACE_WITH_KNOTS((4,2,2,2,2,4),(3,3),(0.0061427298469283,0.00826669470830711,
0.00932436668887678,0.0103820386694465,0.0124973826305858,0.0146213474919646),
(-5.56138389865551E-6,1.00000862090024),.UNSPECIFIED.)
GEOMETRIC_REPRESENTATION_ITEM()
RATIONAL_B_SPLINE_SURFACE(((1.00000326161489,0.706759768337872,1.00000505596145),
(1.00000294808685,0.734947962886857,1.00000456994892),(1.00000271960428,
0.755490020804993,1.00000421576883),(1.00000249159605,0.775989432121355,
1.00000386232404),(1.00000243486463,0.781089952811801,1.00000377438237),
(1.00000236001463,0.787819451077305,1.00000365835434),(1.00000234158974,
0.789475967918561,1.00000362979317),(1.00000234175227,0.789461355654949,
1.00000363004511),(1.00000241511536,0.782865540177451,1.00000374376821),
(1.00000271619448,0.755796583331235,1.00000421048317),(1.0000029464872,
0.735091781130856,1.00000456746925),(1.00000326163462,0.706757994694133,
1.00000505599203)))
REPRESENTATION_ITEM('')
SURFACE()
);
#310=(
BOUNDED_SURFACE()
B_SPLINE_SURFACE(3,2,((#20429,#20430,#20431),(#20432,#20433,#20434),(#20435,
#20436,#20437),(#20438,#20439,#20440),(#20441,#20442,#20443),(#20444,#20445,
#20446),(#20447,#20448,#20449),(#20450,#20451,#20452),(#20453,#20454,#20455),
(#20456,#20457,#20458),(#20459,#20460,#20461),(#20462,#20463,#20464),(#20465,
#20466,#20467),(#20468,#20469,#20470)),.UNSPECIFIED.,.F.,.F.,.F.)
B_SPLINE_SURFACE_WITH_KNOTS((4,2,2,2,2,2,4),(3,3),(2.29850860566927E-17,
0.00228352475280831,0.00342528712921246,0.00456704950561661,0.00570881188202075,
0.0068505742584249,0.00913409901123319),(0.,1.),.UNSPECIFIED.)
GEOMETRIC_REPRESENTATION_ITEM()
RATIONAL_B_SPLINE_SURFACE(((1.,0.755928946018453,1.),(1.,0.755919473251654,
1.),(1.,0.756953933195057,1.),(1.,0.759617125008032,1.),(1.,0.760694585385831,
1.),(1.,0.763054974489942,1.),(1.,0.764326129773376,1.),(1.,0.766864760301965,
1.),(1.,0.768132555731698,1.),(1.,0.770457118175421,1.),(1.,0.77151907153067,
1.),(1.,0.773976852479458,1.),(1.,0.774660609303815,1.),(1.,0.773601014837504,
1.)))
REPRESENTATION_ITEM('')
SURFACE()
);
#311=(
BOUNDED_SURFACE()
B_SPLINE_SURFACE(3,2,((#20547,#20548,#20549),(#20550,#20551,#20552),(#20553,
#20554,#20555),(#20556,#20557,#20558),(#20559,#20560,#20561),(#20562,#20563,
#20564),(#20565,#20566,#20567),(#20568,#20569,#20570),(#20571,#20572,#20573),
(#20574,#20575,#20576),(#20577,#20578,#20579),(#20580,#20581,#20582)),
 .UNSPECIFIED.,.F.,.F.,.F.)
B_SPLINE_SURFACE_WITH_KNOTS((4,2,2,2,2,4),(3,3),(-8.67361737988404E-18,
0.0020019127931021,0.00400382558620421,0.00500478198275526,0.00600573837930632,
0.00800765117240843),(0.,1.),.UNSPECIFIED.)
GEOMETRIC_REPRESENTATION_ITEM()
RATIONAL_B_SPLINE_SURFACE(((1.,0.720245417210284,1.),(1.,0.745456109699134,
1.),(1.,0.776939871169668,1.),(1.,0.843085998617067,1.),(1.,0.876043548544159,
1.),(1.,0.919062364122798,1.),(1.,0.932399541573303,1.),(1.,0.955903426154376,
1.),(1.,0.966062375399352,1.),(1.,0.990944979726916,1.),(1.,1.00003808704948,
1.),(1.,1.,1.)))
REPRESENTATION_ITEM('')
SURFACE()
);
#312=(
BOUNDED_SURFACE()
B_SPLINE_SURFACE(3,2,((#20584,#20585,#20586),(#20587,#20588,#20589),(#20590,
#20591,#20592),(#20593,#20594,#20595),(#20596,#20597,#20598),(#20599,#20600,
#20601),(#20602,#20603,#20604),(#20605,#20606,#20607),(#20608,#20609,#20610),
(#20611,#20612,#20613),(#20614,#20615,#20616),(#20617,#20618,#20619),(#20620,
#20621,#20622),(#20623,#20624,#20625),(#20626,#20627,#20628),(#20629,#20630,
#20631),(#20632,#20633,#20634),(#20635,#20636,#20637)),.UNSPECIFIED.,.F.,
 .F.,.F.)
B_SPLINE_SURFACE_WITH_KNOTS((4,2,2,2,2,2,2,2,4),(3,3),(0.0465879948739151,
0.0488019169422094,0.0499088779763565,0.0510158390105036,0.0532297610787979,
0.054336722112945,0.0554436831470922,0.0598715272836807,0.0642993714202692),
(0.,1.),.UNSPECIFIED.)
GEOMETRIC_REPRESENTATION_ITEM()
RATIONAL_B_SPLINE_SURFACE(((1.,0.720245417210284,1.),(1.,0.715430366769561,
1.),(1.,0.711757488391321,1.),(1.,0.708436125845732,1.),(1.,0.707701704610594,
1.),(1.,0.706997400069913,1.),(1.,0.70703042471459,1.),(1.,0.708269366538293,
1.),(1.,0.710603787640094,1.),(1.,0.716102617085572,1.),(1.,0.718267907422322,
1.),(1.,0.723213640275136,1.),(1.,0.726004552476763,1.),(1.,0.741243869654837,
1.),(1.,0.757174433729962,1.),(1.,0.791690080044701,1.),(1.,0.809643404127687,
1.),(1.,0.826358787974886,1.)))
REPRESENTATION_ITEM('')
SURFACE()
);
#313=(
BOUNDED_SURFACE()
B_SPLINE_SURFACE(3,2,((#20719,#20720,#20721),(#20722,#20723,#20724),(#20725,
#20726,#20727),(#20728,#20729,#20730),(#20731,#20732,#20733),(#20734,#20735,
#20736),(#20737,#20738,#20739),(#20740,#20741,#20742),(#20743,#20744,#20745),
(#20746,#20747,#20748),(#20749,#20750,#20751),(#20752,#20753,#20754),(#20755,
#20756,#20757),(#20758,#20759,#20760),(#20761,#20762,#20763),(#20764,#20765,
#20766)),.UNSPECIFIED.,.F.,.F.,.F.)
B_SPLINE_SURFACE_WITH_KNOTS((4,2,2,2,2,2,2,4),(3,3),(0.00572874702066893,
0.00641318489301232,0.00709762276535571,0.00778206063769909,0.00846649851004248,
0.00915093638238587,0.00983537425472925,0.011204249999416),(0.,1.),
 .UNSPECIFIED.)
GEOMETRIC_REPRESENTATION_ITEM()
RATIONAL_B_SPLINE_SURFACE(((1.,0.975506485486288,1.),(1.,0.975513146220073,
1.),(1.,0.973968479244861,1.),(1.,0.968411518445162,1.),(1.,0.964542733059259,
1.),(1.,0.955226889333692,1.),(1.,0.949822152420214,1.),(1.,0.938073995978702,
1.),(1.,0.931687255706716,1.),(1.,0.918003026598242,1.),(1.,0.91068796451963,
1.),(1.,0.895477555573003,1.),(1.,0.887548913896672,1.),(1.,0.862850245396308,
1.),(1.,0.845167627106926,1.),(1.,0.826358787974873,1.)))
REPRESENTATION_ITEM('')
SURFACE()
);
#314=(
BOUNDED_SURFACE()
B_SPLINE_SURFACE(3,2,((#20852,#20853,#20854),(#20855,#20856,#20857),(#20858,
#20859,#20860),(#20861,#20862,#20863),(#20864,#20865,#20866),(#20867,#20868,
#20869),(#20870,#20871,#20872),(#20873,#20874,#20875),(#20876,#20877,#20878),
(#20879,#20880,#20881),(#20882,#20883,#20884),(#20885,#20886,#20887),(#20888,
#20889,#20890),(#20891,#20892,#20893)),.UNSPECIFIED.,.F.,.F.,.F.)
B_SPLINE_SURFACE_WITH_KNOTS((4,2,2,2,2,2,4),(3,3),(2.29850860566927E-17,
0.00228352475280831,0.00342528712921246,0.0045670495056166,0.00570881188202075,
0.00685057425842489,0.00913409901123318),(0.,1.),.UNSPECIFIED.)
GEOMETRIC_REPRESENTATION_ITEM()
RATIONAL_B_SPLINE_SURFACE(((1.,0.755928946018453,1.),(1.,0.755919473252646,
1.),(1.,0.756953933193741,1.),(1.,0.759617125008685,1.),(1.,0.760694585385853,
1.),(1.,0.763054974489921,1.),(1.,0.764326129773228,1.),(1.,0.766864760302113,
1.),(1.,0.76813255573155,1.),(1.,0.77045711817557,1.),(1.,0.77151907153099,
1.),(1.,0.773976852478821,1.),(1.,0.774660609304298,1.),(1.,0.773601014837506,
1.)))
REPRESENTATION_ITEM('')
SURFACE()
);
#315=(
BOUNDED_SURFACE()
B_SPLINE_SURFACE(3,2,((#20970,#20971,#20972),(#20973,#20974,#20975),(#20976,
#20977,#20978),(#20979,#20980,#20981),(#20982,#20983,#20984),(#20985,#20986,
#20987),(#20988,#20989,#20990),(#20991,#20992,#20993),(#20994,#20995,#20996),
(#20997,#20998,#20999),(#21000,#21001,#21002),(#21003,#21004,#21005),(#21006,
#21007,#21008),(#21009,#21010,#21011)),.UNSPECIFIED.,.F.,.F.,.F.)
B_SPLINE_SURFACE_WITH_KNOTS((4,2,2,2,2,2,4),(3,3),(0.0025838157606072,0.0039611177618176,
0.005338419763028,0.0060270707636332,0.0067157217642384,0.0074043727648436,
0.0080930237654488),(0.,1.),.UNSPECIFIED.)
GEOMETRIC_REPRESENTATION_ITEM()
RATIONAL_B_SPLINE_SURFACE(((1.,0.826358787974881,1.),(1.,0.845245405300955,
1.),(1.,0.862939160435579,1.),(1.,0.895803497327567,1.),(1.,0.91098843375652,
1.),(1.,0.931602584770477,1.),(1.,0.938050525530194,1.),(1.,0.949865147477405,
1.),(1.,0.95528172500017,1.),(1.,0.964523416337373,1.),(1.,0.96840980801867,
1.),(1.,0.973963943287705,1.),(1.,0.975504577407296,1.),(1.,0.975506485486285,
1.)))
REPRESENTATION_ITEM('')
SURFACE()
);
#316=(
BOUNDED_SURFACE()
B_SPLINE_SURFACE(3,2,((#21013,#21014,#21015),(#21016,#21017,#21018),(#21019,
#21020,#21021),(#21022,#21023,#21024),(#21025,#21026,#21027),(#21028,#21029,
#21030),(#21031,#21032,#21033),(#21034,#21035,#21036),(#21037,#21038,#21039),
(#21040,#21041,#21042),(#21043,#21044,#21045),(#21046,#21047,#21048)),
 .UNSPECIFIED.,.F.,.F.,.F.)
B_SPLINE_SURFACE_WITH_KNOTS((4,2,2,2,2,4),(3,3),(6.93889390390723E-18,0.00200191279310211,
0.00400382558620421,0.00500478198275526,0.00600573837930631,0.00800765117240842),
(0.,1.),.UNSPECIFIED.)
GEOMETRIC_REPRESENTATION_ITEM()
RATIONAL_B_SPLINE_SURFACE(((1.,0.72024541721028,1.),(1.,0.745456109696734,
1.),(1.,0.776939871172863,1.),(1.,0.843085998613875,1.),(1.,0.876043548543787,
1.),(1.,0.919062364122984,1.),(1.,0.932399541573454,1.),(1.,0.955903426154228,
1.),(1.,0.966062375399276,1.),(1.,0.990944979727062,1.),(1.,1.00003808704937,
1.),(1.,1.,1.)))
REPRESENTATION_ITEM('')
SURFACE()
);
#317=(
BOUNDED_SURFACE()
B_SPLINE_SURFACE(3,2,((#21050,#21051,#21052),(#21053,#21054,#21055),(#21056,
#21057,#21058),(#21059,#21060,#21061),(#21062,#21063,#21064),(#21065,#21066,
#21067),(#21068,#21069,#21070),(#21071,#21072,#21073),(#21074,#21075,#21076),
(#21077,#21078,#21079),(#21080,#21081,#21082),(#21083,#21084,#21085),(#21086,
#21087,#21088),(#21089,#21090,#21091),(#21092,#21093,#21094),(#21095,#21096,
#21097),(#21098,#21099,#21100),(#21101,#21102,#21103),(#21104,#21105,#21106),
(#21107,#21108,#21109),(#21110,#21111,#21112),(#21113,#21114,#21115)),
 .UNSPECIFIED.,.F.,.F.,.F.)
B_SPLINE_SURFACE_WITH_KNOTS((4,2,2,2,2,2,2,2,2,2,4),(3,3),(0.0436602992904701,
0.0480963033926944,0.0491980653433177,0.050299827293941,0.0514015892445644,
0.0525033511951877,0.0547068750964343,0.0558086370470577,0.056910398997681,
0.0591139228989276,0.0613234933874712),(0.,1.00002895629973),
 .UNSPECIFIED.)
GEOMETRIC_REPRESENTATION_ITEM()
RATIONAL_B_SPLINE_SURFACE(((1.,0.826683641938831,1.00001003720082),(1.,
0.809845600472633,1.00001101233558),(1.,0.79184731214926,1.00001205466324),
(1.,0.770216550347386,1.00001330735688),(1.,0.765954721069219,1.00001355417049),
(1.,0.757698677929212,1.00001403229941),(1.,0.753690542776134,1.00001426442094),
(1.,0.745987105952188,1.00001471054699),(1.,0.742291755413244,1.00001492455435),
(1.,0.735294059977715,1.00001532980908),(1.,0.731982797792345,1.00001552157288),
(1.,0.722886163295819,1.00001604838263),(1.,0.71790361921332,1.00001633693471),
(1.,0.712405002570856,1.00001665537389),(1.,0.710901207883209,1.00001674246255),
(1.,0.708608218307941,1.00001687525554),(1.,0.707818554135303,1.00001692098704),
(1.,0.706612720262668,1.00001699082002),(1.,0.707341409991791,1.0000169486197),
(1.,0.711697151558445,1.00001669636739),(1.,0.715335875779425,1.00001648563941),
(1.,0.720277859138149,1.0000161994363)))
REPRESENTATION_ITEM('')
SURFACE()
);
#318=(
BOUNDED_SURFACE()
B_SPLINE_SURFACE(2,2,((#22381,#22382,#22383),(#22384,#22385,#22386),(#22387,
#22388,#22389),(#22390,#22391,#22392),(#22393,#22394,#22395),(#22396,#22397,
#22398),(#22399,#22400,#22401),(#22402,#22403,#22404),(#22405,#22406,#22407)),
 .UNSPECIFIED.,.T.,.F.,.F.)
B_SPLINE_SURFACE_WITH_KNOTS((3,2,2,2,3),(3,3),(-3.14159265358979,-1.5707963267949,
0.,1.5707963267949,3.14159265358979),(-2.35619449019236,-0.785398163397175),
 .UNSPECIFIED.)
GEOMETRIC_REPRESENTATION_ITEM()
RATIONAL_B_SPLINE_SURFACE(((1.,0.707106781186444,1.),(0.707106781186499,
0.499999999999893,0.707106781186499),(1.,0.707106781186444,1.),(0.707106781186553,
0.499999999999931,0.707106781186553),(1.,0.707106781186444,1.),(0.707106781186499,
0.499999999999893,0.707106781186499),(1.,0.707106781186444,1.),(0.707106781186553,
0.499999999999931,0.707106781186553),(1.,0.707106781186444,1.)))
REPRESENTATION_ITEM('')
SURFACE()
);
#319=(
BOUNDED_SURFACE()
B_SPLINE_SURFACE(2,2,((#22408,#22409,#22410),(#22411,#22412,#22413),(#22414,
#22415,#22416),(#22417,#22418,#22419),(#22420,#22421,#22422),(#22423,#22424,
#22425),(#22426,#22427,#22428),(#22429,#22430,#22431),(#22432,#22433,#22434)),
 .UNSPECIFIED.,.T.,.F.,.F.)
B_SPLINE_SURFACE_WITH_KNOTS((3,2,2,2,3),(3,3),(-3.14159265358979,-1.5707963267949,
0.,1.5707963267949,3.14159265358979),(-2.35619449019277,-0.785398163397194),
 .UNSPECIFIED.)
GEOMETRIC_REPRESENTATION_ITEM()
RATIONAL_B_SPLINE_SURFACE(((1.,0.707106781186307,1.),(0.707106781186516,
0.499999999999808,0.707106781186516),(1.,0.707106781186307,1.),(0.707106781186497,
0.499999999999794,0.707106781186497),(1.,0.707106781186307,1.),(0.707106781186516,
0.499999999999808,0.707106781186516),(1.,0.707106781186307,1.),(0.707106781186497,
0.499999999999794,0.707106781186497),(1.,0.707106781186307,1.)))
REPRESENTATION_ITEM('')
SURFACE()
);
#320=(
BOUNDED_SURFACE()
B_SPLINE_SURFACE(2,2,((#22485,#22486,#22487),(#22488,#22489,#22490),(#22491,
#22492,#22493),(#22494,#22495,#22496),(#22497,#22498,#22499),(#22500,#22501,
#22502),(#22503,#22504,#22505),(#22506,#22507,#22508),(#22509,#22510,#22511)),
 .UNSPECIFIED.,.T.,.F.,.F.)
B_SPLINE_SURFACE_WITH_KNOTS((3,2,2,2,3),(3,3),(-3.14159265358979,-1.5707963267949,
0.,1.5707963267949,3.14159265358979),(-2.35619449019236,-0.785398163397439),
 .UNSPECIFIED.)
GEOMETRIC_REPRESENTATION_ITEM()
RATIONAL_B_SPLINE_SURFACE(((1.,0.707106781186539,1.),(0.707106781186531,
0.499999999999982,0.707106781186531),(1.,0.707106781186539,1.),(0.707106781186538,
0.499999999999987,0.707106781186538),(1.,0.707106781186539,1.),(0.707106781186531,
0.499999999999982,0.707106781186531),(1.,0.707106781186539,1.),(0.707106781186538,
0.499999999999987,0.707106781186538),(1.,0.707106781186539,1.)))
REPRESENTATION_ITEM('')
SURFACE()
);
#321=(
BOUNDED_SURFACE()
B_SPLINE_SURFACE(2,2,((#22512,#22513,#22514),(#22515,#22516,#22517),(#22518,
#22519,#22520),(#22521,#22522,#22523),(#22524,#22525,#22526),(#22527,#22528,
#22529),(#22530,#22531,#22532),(#22533,#22534,#22535),(#22536,#22537,#22538)),
 .UNSPECIFIED.,.T.,.F.,.F.)
B_SPLINE_SURFACE_WITH_KNOTS((3,2,2,2,3),(3,3),(-3.14159265358979,-1.5707963267949,
0.,1.5707963267949,3.14159265358979),(-2.35619449019241,-0.785398163397432),
 .UNSPECIFIED.)
GEOMETRIC_REPRESENTATION_ITEM()
RATIONAL_B_SPLINE_SURFACE(((1.,0.707106781186519,1.),(0.707106781186627,
0.500000000000036,0.707106781186627),(1.,0.707106781186519,1.),(0.707106781186571,
0.499999999999996,0.707106781186571),(1.,0.707106781186519,1.),(0.707106781186627,
0.500000000000036,0.707106781186627),(1.,0.707106781186519,1.),(0.707106781186571,
0.499999999999996,0.707106781186571),(1.,0.707106781186519,1.)))
REPRESENTATION_ITEM('')
SURFACE()
);
#322=(
BOUNDED_SURFACE()
B_SPLINE_SURFACE(3,2,((#23001,#23002,#23003),(#23004,#23005,#23006),(#23007,
#23008,#23009),(#23010,#23011,#23012),(#23013,#23014,#23015),(#23016,#23017,
#23018),(#23019,#23020,#23021),(#23022,#23023,#23024),(#23025,#23026,#23027),
(#23028,#23029,#23030),(#23031,#23032,#23033),(#23034,#23035,#23036),(#23037,
#23038,#23039),(#23040,#23041,#23042),(#23043,#23044,#23045),(#23046,#23047,
#23048),(#23049,#23050,#23051),(#23052,#23053,#23054),(#23055,#23056,#23057),
(#23058,#23059,#23060),(#23061,#23062,#23063),(#23064,#23065,#23066),(#23067,
#23068,#23069),(#23070,#23071,#23072),(#23073,#23074,#23075),(#23076,#23077,
#23078),(#23079,#23080,#23081),(#23082,#23083,#23084),(#23085,#23086,#23087),
(#23088,#23089,#23090),(#23091,#23092,#23093),(#23094,#23095,#23096),(#23097,
#23098,#23099),(#23100,#23101,#23102),(#23103,#23104,#23105),(#23106,#23107,
#23108),(#23109,#23110,#23111),(#23112,#23113,#23114),(#23115,#23116,#23117),
(#23118,#23119,#23120),(#23121,#23122,#23123),(#23124,#23125,#23126),(#23127,
#23128,#23129),(#23130,#23131,#23132),(#23133,#23134,#23135),(#23136,#23137,
#23138),(#23139,#23140,#23141),(#23142,#23143,#23144),(#23145,#23146,#23147),
(#23148,#23149,#23150),(#23151,#23152,#23153),(#23154,#23155,#23156),(#23157,
#23158,#23159),(#23160,#23161,#23162)),.UNSPECIFIED.,.F.,.F.,.F.)
B_SPLINE_SURFACE_WITH_KNOTS((4,2,2,2,2,2,2,2,2,2,2,2,2,2,2,2,2,2,2,2,2,
2,2,2,2,2,4),(3,3),(0.0156830691858876,0.0164505202472942,0.0166981564596516,
0.0171934288843663,0.017688701309081,0.0181839737337957,0.0191745185832252,
0.0201650634326547,0.0221461531315136,0.0241272428303725,0.025117787679802,
0.0261083325292314,0.0280894222280904,0.0300705119269493,0.0320516016258082,
0.0360137810235261,0.037994870722385,0.0399759604212439,0.0419570501201028,
0.0439381398189618,0.0449286846683912,0.0459192295178207,0.0464145019425354,
0.0469097743672502,0.0474050467919649,0.0476526830043223,0.0484205987519554),
(-0.000176656774630185,1.00140559977643),.UNSPECIFIED.)
GEOMETRIC_REPRESENTATION_ITEM()
RATIONAL_B_SPLINE_SURFACE(((1.00000185229478,0.994749992386749,1.00001475620861),
(1.00000110311236,0.996873419742612,1.0000087878864),(1.00000061689249,
0.998251525466236,1.00000491444144),(1.00000073022143,0.99793031426867,
1.0000058172705),(1.00000081643938,0.997685944476427,1.00000650412124),
(1.00000116817153,0.996689020835744,1.00000930617684),(1.00000151293943,
0.995711836146633,1.00001205275212),(1.00000222875737,0.99368297460525,
1.00001775527797),(1.00000261226297,0.992595994639531,1.00002081045509),
(1.00000339798395,0.990369005078046,1.00002706985983),(1.00000379540439,
0.989242585902711,1.00003023588883),(1.00000499052043,0.985855237206275,
1.00003975671769),(1.00000579086045,0.983586812540499,1.00004613258417),
(1.00000737677408,0.97909181598218,1.00005876668146),(1.00000816422513,
0.976859922850868,1.00006503986867),(1.00001048220609,0.970290008684874,
1.0000835059417),(1.0000119461136,0.966140817279626,1.00009516808364),(1.00001468654717,
0.958373534637283,1.00011699960303),(1.00001596349836,0.954754238433,1.00012717236729),
(1.00001771880672,0.949779121960846,1.00014115593873),(1.00001827868632,
0.948192240535891,1.00014561619005),(1.00001932722233,0.945220347466773,
1.00015396929681),(1.00001981740926,0.943830997788028,1.00015787434518),
(1.00002118448659,0.939956254724288,1.00016876509453),(1.00002195823644,
0.937763195243397,1.00017492913191),(1.00002321565211,0.934199269074837,
1.00018494626748),(1.00002370061483,0.932824726524174,1.00018880969743),
(1.00002434501334,0.930998290964812,1.00019394326411),(1.00002450689124,
0.930539476192181,1.00019523285585),(1.00002450200607,0.930553322329606,
1.00019519393848),(1.00002385083742,0.932398946709429,1.00019000643775),
(1.00002196617021,0.937740708359039,1.00017499233585),(1.00002117811911,
0.939974302221974,1.00016871436838),(1.00001935011025,0.945155475621783,
1.00015415163226),(1.00001830824342,0.948108466066406,1.00014585165514),
(1.00001599049957,0.954677708176843,1.00012738747106),(1.0000147145338,
0.958294211383293,1.00011722255709),(1.00001194082592,0.966155804298885,
1.00009512595959),(1.00001046725737,0.97033237824493,1.00008338685348),
(1.00000815970583,0.976872732002048,1.00006500386596),(1.00000737308074,
0.979102284123733,1.00005873725863),(1.00000577774524,0.983623985306201,
1.0000460281026),(1.00000497387877,0.985902405097253,1.00003962414279),
(1.000003776533,0.989296073600137,1.00003008555083),(1.00000337746495,0.990427162612735,
1.00002690639631),(1.00000259754195,0.992637718792777,1.00002069318092),
(1.00000221666145,0.993717258376601,1.0000176589165),(1.00000150078254,
0.995746292719822,1.00001195590495),(1.00000115795301,0.996717983459339,
1.00000922477153),(1.00000081463085,0.997691070447167,1.00000648971367),
(1.00000072988353,0.997931272000135,1.0000058145786),(1.00000061781061,
0.99824892319208,1.00000492175566),(1.00000109047742,0.996909231281611,
1.00000868723083),(1.00000189977857,0.994615407843422,1.0000151344857)))
REPRESENTATION_ITEM('')
SURFACE()
);
#323=(
BOUNDED_SURFACE()
B_SPLINE_SURFACE(1,2,((#25031,#25032,#25033,#25034,#25035,#25036,#25037,
#25038,#25039,#25040,#25041,#25042,#25043,#25044,#25045,#25046,#25047,#25048,
#25049,#25050,#25051,#25052,#25053,#25054,#25055,#25056,#25057,#25058,#25059,
#25060,#25061,#25062,#25063,#25064,#25065,#25066,#25067,#25068,#25069,#25070,
#25071,#25072,#25073,#25074,#25075,#25076,#25077,#25078,#25079,#25080,#25081,
#25082,#25083,#25084,#25085,#25086,#25087,#25088,#25089,#25090,#25091,#25092,
#25093,#25094,#25095,#25096,#25097,#25098,#25099,#25100,#25101,#25102,#25103,
#25104,#25105,#25106,#25107,#25108,#25109,#25110,#25111,#25112,#25113,#25114,
#25115,#25116,#25117,#25118,#25119,#25120,#25121,#25122,#25123,#25124,#25125,
#25126,#25127,#25128,#25129,#25130,#25131,#25132,#25133,#25134,#25135,#25136,
#25137,#25138,#25139,#25140,#25141,#25142,#25143,#25144,#25145,#25146,#25147,
#25148,#25149,#25150,#25151,#25152,#25153,#25154,#25155,#25156,#25157,#25158,
#25159,#25160,#25161,#25162,#25163,#25164,#25165,#25166,#25167,#25168,#25169,
#25170,#25171,#25172,#25173,#25174,#25175,#25176,#25177,#25178,#25179,#25180,
#25181,#25182,#25183,#25184,#25185,#25186,#25187,#25188,#25189,#25190,#25191,
#25192,#25193,#25194,#25195,#25196,#25197,#25198,#25199,#25200,#25201,#25202,
#25203,#25204,#25205,#25206,#25207,#25208,#25209,#25210,#25211,#25212,#25213,
#25214,#25215,#25216,#25217,#25218,#25219,#25220,#25221,#25222,#25223,#25224,
#25225,#25226,#25227,#25228,#25229,#25230,#25231,#25232,#25233,#25234,#25235,
#25236,#25237,#25238,#25239,#25240,#25241,#25242,#25243,#25244,#25245,#25246,
#25247,#25248,#25249,#25250,#25251,#25252,#25253,#25254,#25255),(#25256,
#25257,#25258,#25259,#25260,#25261,#25262,#25263,#25264,#25265,#25266,#25267,
#25268,#25269,#25270,#25271,#25272,#25273,#25274,#25275,#25276,#25277,#25278,
#25279,#25280,#25281,#25282,#25283,#25284,#25285,#25286,#25287,#25288,#25289,
#25290,#25291,#25292,#25293,#25294,#25295,#25296,#25297,#25298,#25299,#25300,
#25301,#25302,#25303,#25304,#25305,#25306,#25307,#25308,#25309,#25310,#25311,
#25312,#25313,#25314,#25315,#25316,#25317,#25318,#25319,#25320,#25321,#25322,
#25323,#25324,#25325,#25326,#25327,#25328,#25329,#25330,#25331,#25332,#25333,
#25334,#25335,#25336,#25337,#25338,#25339,#25340,#25341,#25342,#25343,#25344,
#25345,#25346,#25347,#25348,#25349,#25350,#25351,#25352,#25353,#25354,#25355,
#25356,#25357,#25358,#25359,#25360,#25361,#25362,#25363,#25364,#25365,#25366,
#25367,#25368,#25369,#25370,#25371,#25372,#25373,#25374,#25375,#25376,#25377,
#25378,#25379,#25380,#25381,#25382,#25383,#25384,#25385,#25386,#25387,#25388,
#25389,#25390,#25391,#25392,#25393,#25394,#25395,#25396,#25397,#25398,#25399,
#25400,#25401,#25402,#25403,#25404,#25405,#25406,#25407,#25408,#25409,#25410,
#25411,#25412,#25413,#25414,#25415,#25416,#25417,#25418,#25419,#25420,#25421,
#25422,#25423,#25424,#25425,#25426,#25427,#25428,#25429,#25430,#25431,#25432,
#25433,#25434,#25435,#25436,#25437,#25438,#25439,#25440,#25441,#25442,#25443,
#25444,#25445,#25446,#25447,#25448,#25449,#25450,#25451,#25452,#25453,#25454,
#25455,#25456,#25457,#25458,#25459,#25460,#25461,#25462,#25463,#25464,#25465,
#25466,#25467,#25468,#25469,#25470,#25471,#25472,#25473,#25474,#25475,#25476,
#25477,#25478,#25479,#25480)),.UNSPECIFIED.,.F.,.F.,.F.)
B_SPLINE_SURFACE_WITH_KNOTS((2,2),(3,2,2,2,2,2,2,2,2,2,2,2,2,2,2,2,2,2,
2,2,2,2,2,2,2,2,2,2,2,2,2,2,2,2,2,2,2,2,2,2,2,2,2,2,2,2,2,2,2,2,2,2,2,2,
2,2,2,2,2,2,2,2,2,2,2,2,2,2,2,2,2,2,2,2,2,2,2,2,2,2,2,2,2,2,2,2,2,2,2,2,
2,2,2,2,2,2,2,2,2,2,2,2,2,2,2,2,2,2,2,2,2,2,3),(0.,1.00000154805557),(0.,
0.00892857142857143,0.0178571428571429,0.0267857142857143,0.0357142857142857,
0.0446428571428571,0.0535714285714286,0.0625,0.0714285714285714,0.0803571428571429,
0.0892857142857143,0.0982142857142857,0.107142857142857,0.116071428571429,
0.125,0.133928571428571,0.142857142857143,0.151785714285714,0.160714285714286,
0.169642857142857,0.178571428571429,0.1875,0.196428571428571,0.205357142857143,
0.214285714285714,0.223214285714286,0.232142857142857,0.241071428571429,
0.25,0.258928571428571,0.267857142857143,0.276785714285714,0.285714285714286,
0.294642857142857,0.303571428571429,0.3125,0.321428571428571,0.330357142857143,
0.339285714285714,0.348214285714286,0.357142857142857,0.366071428571429,
0.375,0.383928571428571,0.392857142857143,0.401785714285714,0.410714285714286,
0.419642857142857,0.428571428571429,0.4375,0.446428571428571,0.455357142857143,
0.464285714285714,0.473214285714286,0.482142857142857,0.491071428571429,
0.5,0.508928571428571,0.517857142857143,0.526785714285714,0.535714285714286,
0.544642857142857,0.553571428571429,0.5625,0.571428571428571,0.580357142857143,
0.589285714285714,0.598214285714286,0.607142857142857,0.616071428571429,
0.625,0.633928571428571,0.642857142857143,0.651785714285714,0.660714285714286,
0.669642857142857,0.678571428571429,0.6875,0.696428571428571,0.705357142857143,
0.714285714285714,0.723214285714286,0.732142857142857,0.741071428571429,
0.75,0.758928571428571,0.767857142857143,0.776785714285714,0.785714285714286,
0.794642857142857,0.803571428571429,0.8125,0.821428571428571,0.830357142857143,
0.839285714285714,0.848214285714286,0.857142857142857,0.866071428571429,
0.875,0.883928571428571,0.892857142857143,0.901785714285714,0.910714285714286,
0.919642857142857,0.928571428571429,0.9375,0.946428571428571,0.955357142857143,
0.964285714285714,0.973214285714286,0.982142857142857,0.991071428571429,
1.),.UNSPECIFIED.)
GEOMETRIC_REPRESENTATION_ITEM()
RATIONAL_B_SPLINE_SURFACE(((1.,0.923879532511287,1.,0.923879532511287,1.,
0.923879532511287,1.,0.923879532511287,1.,0.923879532511287,1.,0.923879532511287,
1.,0.923879532511287,1.,0.923879532511287,1.,0.923879532511287,1.,0.923879532511287,
1.,0.923879532511287,1.,0.923879532511287,1.,0.923879532511287,1.,0.923879532511287,
1.,0.923879532511287,1.,0.923879532511287,1.,0.923879532511287,1.,0.923879532511287,
1.,0.923879532511287,1.,0.923879532511287,1.,0.923879532511287,1.,0.923879532511287,
1.,0.923879532511287,1.,0.923879532511287,1.,0.923879532511287,1.,0.923879532511287,
1.,0.923879532511287,1.,0.923879532511287,1.,0.923879532511287,1.,0.923879532511287,
1.,0.923879532511287,1.,0.923879532511287,1.,0.923879532511287,1.,0.923879532511287,
1.,0.923879532511287,1.,0.923879532511287,1.,0.923879532511287,1.,0.923879532511287,
1.,0.923879532511287,1.,0.923879532511287,1.,0.923879532511287,1.,0.923879532511287,
1.,0.923879532511287,1.,0.923879532511287,1.,0.923879532511287,1.,0.923879532511287,
1.,0.923879532511287,1.,0.923879532511287,1.,0.923879532511287,1.,0.923879532511287,
1.,0.923879532511287,1.,0.923879532511287,1.,0.923879532511287,1.,0.923879532511287,
1.,0.923879532511287,1.,0.923879532511287,1.,0.923879532511287,1.,0.923879532511287,
1.,0.923879532511287,1.,0.923879532511287,1.,0.923879532511287,1.,0.923879532511287,
1.,0.923879532511287,1.,0.923879532511287,1.,0.923879532511287,1.,0.923879532511287,
1.,0.923879532511287,1.,0.923879532511287,1.,0.923879532511287,1.,0.923879532511287,
1.,0.923879532511287,1.,0.923879532511287,1.,0.923879532511287,1.,0.923879532511287,
1.,0.923879532511287,1.,0.923879532511287,1.,0.923879532511287,1.,0.923879532511287,
1.,0.923879532511287,1.,0.923879532511287,1.,0.923879532511287,1.,0.923879532511287,
1.,0.923879532511287,1.,0.923879532511287,1.,0.923879532511287,1.,0.923879532511287,
1.,0.923879532511287,1.,0.923879532511287,1.,0.923879532511287,1.,0.923879532511287,
1.,0.923879532511287,1.,0.923879532511287,1.,0.923879532511287,1.,0.923879532511287,
1.,0.923879532511287,1.,0.923879532511287,1.,0.923879532511287,1.,0.923879532511287,
1.,0.923879532511287,1.,0.923879532511287,1.,0.923879532511287,1.,0.923879532511287,
1.,0.923879532511287,1.,0.923879532511287,1.,0.923879532511287,1.,0.923879532511287,
1.,0.923879532511287,1.,0.923879532511287,1.,0.923879532511287,1.,0.923879532511287,
1.,0.923879532511287,1.,0.923879532511287,1.),(1.,0.923879532511287,1.,
0.923879532511287,1.,0.923879532511287,1.,0.923879532511287,1.,0.923879532511287,
1.,0.923879532511287,1.,0.923879532511287,1.,0.923879532511287,1.,0.923879532511287,
1.,0.923879532511287,1.,0.923879532511287,1.,0.923879532511287,1.,0.923879532511287,
1.,0.923879532511287,1.,0.923879532511287,1.,0.923879532511287,1.,0.923879532511287,
1.,0.923879532511287,1.,0.923879532511287,1.,0.923879532511287,1.,0.923879532511287,
1.,0.923879532511287,1.,0.923879532511287,1.,0.923879532511287,1.,0.923879532511287,
1.,0.923879532511287,1.,0.923879532511287,1.,0.923879532511287,1.,0.923879532511287,
1.,0.923879532511287,1.,0.923879532511287,1.,0.923879532511287,1.,0.923879532511287,
1.,0.923879532511287,1.,0.923879532511287,1.,0.923879532511287,1.,0.923879532511287,
1.,0.923879532511287,1.,0.923879532511287,1.,0.923879532511287,1.,0.923879532511287,
1.,0.923879532511287,1.,0.923879532511287,1.,0.923879532511287,1.,0.923879532511287,
1.,0.923879532511287,1.,0.923879532511287,1.,0.923879532511287,1.,0.923879532511287,
1.,0.923879532511287,1.,0.923879532511287,1.,0.923879532511287,1.,0.923879532511287,
1.,0.923879532511287,1.,0.923879532511287,1.,0.923879532511287,1.,0.923879532511287,
1.,0.923879532511287,1.,0.923879532511287,1.,0.923879532511287,1.,0.923879532511287,
1.,0.923879532511287,1.,0.923879532511287,1.,0.923879532511287,1.,0.923879532511287,
1.,0.923879532511287,1.,0.923879532511287,1.,0.923879532511287,1.,0.923879532511287,
1.,0.923879532511287,1.,0.923879532511287,1.,0.923879532511287,1.,0.923879532511287,
1.,0.923879532511287,1.,0.923879532511287,1.,0.923879532511287,1.,0.923879532511287,
1.,0.923879532511287,1.,0.923879532511287,1.,0.923879532511287,1.,0.923879532511287,
1.,0.923879532511287,1.,0.923879532511287,1.,0.923879532511287,1.,0.923879532511287,
1.,0.923879532511287,1.,0.923879532511287,1.,0.923879532511287,1.,0.923879532511287,
1.,0.923879532511287,1.,0.923879532511287,1.,0.923879532511287,1.,0.923879532511287,
1.,0.923879532511287,1.,0.923879532511287,1.,0.923879532511287,1.,0.923879532511287,
1.,0.923879532511287,1.,0.923879532511287,1.,0.923879532511287,1.,0.923879532511287,
1.,0.923879532511287,1.,0.923879532511287,1.,0.923879532511287,1.,0.923879532511287,
1.,0.923879532511287,1.,0.923879532511287,1.,0.923879532511287,1.,0.923879532511287,
1.,0.923879532511287,1.,0.923879532511287,1.,0.923879532511287,1.)))
REPRESENTATION_ITEM('')
SURFACE()
);
#324=(
BOUNDED_SURFACE()
B_SPLINE_SURFACE(1,2,((#25500,#25501,#25502,#25503,#25504,#25505,#25506,
#25507,#25508,#25509,#25510,#25511,#25512,#25513,#25514,#25515,#25516,#25517,
#25518,#25519,#25520,#25521,#25522,#25523,#25524,#25525,#25526,#25527,#25528,
#25529,#25530,#25531,#25532,#25533,#25534,#25535,#25536,#25537,#25538,#25539,
#25540,#25541,#25542,#25543,#25544,#25545,#25546,#25547,#25548,#25549,#25550,
#25551,#25552,#25553,#25554,#25555,#25556,#25557,#25558,#25559,#25560,#25561,
#25562,#25563,#25564,#25565,#25566,#25567,#25568,#25569,#25570,#25571,#25572,
#25573,#25574,#25575,#25576,#25577,#25578,#25579,#25580,#25581,#25582,#25583,
#25584,#25585,#25586,#25587,#25588,#25589,#25590,#25591,#25592,#25593,#25594,
#25595,#25596,#25597,#25598,#25599,#25600,#25601,#25602,#25603,#25604,#25605,
#25606,#25607,#25608,#25609,#25610,#25611,#25612,#25613,#25614,#25615,#25616,
#25617,#25618,#25619,#25620,#25621,#25622,#25623,#25624,#25625,#25626,#25627,
#25628,#25629,#25630,#25631,#25632,#25633,#25634,#25635,#25636,#25637,#25638,
#25639,#25640,#25641,#25642,#25643,#25644,#25645,#25646,#25647,#25648,#25649,
#25650,#25651,#25652,#25653,#25654,#25655,#25656,#25657,#25658,#25659,#25660,
#25661,#25662,#25663,#25664,#25665,#25666,#25667,#25668,#25669,#25670,#25671,
#25672,#25673,#25674,#25675,#25676,#25677,#25678,#25679,#25680,#25681,#25682,
#25683,#25684,#25685,#25686,#25687,#25688,#25689,#25690,#25691,#25692,#25693,
#25694,#25695,#25696,#25697,#25698,#25699,#25700,#25701,#25702,#25703,#25704,
#25705,#25706,#25707,#25708,#25709,#25710,#25711,#25712,#25713,#25714,#25715,
#25716,#25717,#25718,#25719,#25720,#25721,#25722,#25723,#25724),(#25725,
#25726,#25727,#25728,#25729,#25730,#25731,#25732,#25733,#25734,#25735,#25736,
#25737,#25738,#25739,#25740,#25741,#25742,#25743,#25744,#25745,#25746,#25747,
#25748,#25749,#25750,#25751,#25752,#25753,#25754,#25755,#25756,#25757,#25758,
#25759,#25760,#25761,#25762,#25763,#25764,#25765,#25766,#25767,#25768,#25769,
#25770,#25771,#25772,#25773,#25774,#25775,#25776,#25777,#25778,#25779,#25780,
#25781,#25782,#25783,#25784,#25785,#25786,#25787,#25788,#25789,#25790,#25791,
#25792,#25793,#25794,#25795,#25796,#25797,#25798,#25799,#25800,#25801,#25802,
#25803,#25804,#25805,#25806,#25807,#25808,#25809,#25810,#25811,#25812,#25813,
#25814,#25815,#25816,#25817,#25818,#25819,#25820,#25821,#25822,#25823,#25824,
#25825,#25826,#25827,#25828,#25829,#25830,#25831,#25832,#25833,#25834,#25835,
#25836,#25837,#25838,#25839,#25840,#25841,#25842,#25843,#25844,#25845,#25846,
#25847,#25848,#25849,#25850,#25851,#25852,#25853,#25854,#25855,#25856,#25857,
#25858,#25859,#25860,#25861,#25862,#25863,#25864,#25865,#25866,#25867,#25868,
#25869,#25870,#25871,#25872,#25873,#25874,#25875,#25876,#25877,#25878,#25879,
#25880,#25881,#25882,#25883,#25884,#25885,#25886,#25887,#25888,#25889,#25890,
#25891,#25892,#25893,#25894,#25895,#25896,#25897,#25898,#25899,#25900,#25901,
#25902,#25903,#25904,#25905,#25906,#25907,#25908,#25909,#25910,#25911,#25912,
#25913,#25914,#25915,#25916,#25917,#25918,#25919,#25920,#25921,#25922,#25923,
#25924,#25925,#25926,#25927,#25928,#25929,#25930,#25931,#25932,#25933,#25934,
#25935,#25936,#25937,#25938,#25939,#25940,#25941,#25942,#25943,#25944,#25945,
#25946,#25947,#25948,#25949)),.UNSPECIFIED.,.F.,.F.,.F.)
B_SPLINE_SURFACE_WITH_KNOTS((2,2),(3,2,2,2,2,2,2,2,2,2,2,2,2,2,2,2,2,2,
2,2,2,2,2,2,2,2,2,2,2,2,2,2,2,2,2,2,2,2,2,2,2,2,2,2,2,2,2,2,2,2,2,2,2,2,
2,2,2,2,2,2,2,2,2,2,2,2,2,2,2,2,2,2,2,2,2,2,2,2,2,2,2,2,2,2,2,2,2,2,2,2,
2,2,2,2,2,2,2,2,2,2,2,2,2,2,2,2,2,2,2,2,2,2,3),(0.,1.),(0.,0.00892857142857143,
0.0178571428571429,0.0267857142857143,0.0357142857142857,0.0446428571428571,
0.0535714285714286,0.0625,0.0714285714285714,0.0803571428571429,0.0892857142857143,
0.0982142857142857,0.107142857142857,0.116071428571429,0.125,0.133928571428571,
0.142857142857143,0.151785714285714,0.160714285714286,0.169642857142857,
0.178571428571429,0.1875,0.196428571428571,0.205357142857143,0.214285714285714,
0.223214285714286,0.232142857142857,0.241071428571429,0.25,0.258928571428571,
0.267857142857143,0.276785714285714,0.285714285714286,0.294642857142857,
0.303571428571429,0.3125,0.321428571428571,0.330357142857143,0.339285714285714,
0.348214285714286,0.357142857142857,0.366071428571429,0.375,0.383928571428571,
0.392857142857143,0.401785714285714,0.410714285714286,0.419642857142857,
0.428571428571429,0.4375,0.446428571428571,0.455357142857143,0.464285714285714,
0.473214285714286,0.482142857142857,0.491071428571429,0.5,0.508928571428571,
0.517857142857143,0.526785714285714,0.535714285714286,0.544642857142857,
0.553571428571429,0.5625,0.571428571428571,0.580357142857143,0.589285714285714,
0.598214285714286,0.607142857142857,0.616071428571429,0.625,0.633928571428571,
0.642857142857143,0.651785714285714,0.660714285714286,0.669642857142857,
0.678571428571429,0.6875,0.696428571428571,0.705357142857143,0.714285714285714,
0.723214285714286,0.732142857142857,0.741071428571429,0.75,0.758928571428571,
0.767857142857143,0.776785714285714,0.785714285714286,0.794642857142857,
0.803571428571429,0.8125,0.821428571428571,0.830357142857143,0.839285714285714,
0.848214285714286,0.857142857142857,0.866071428571429,0.875,0.883928571428571,
0.892857142857143,0.901785714285714,0.910714285714286,0.919642857142857,
0.928571428571429,0.9375,0.946428571428571,0.955357142857143,0.964285714285714,
0.973214285714286,0.982142857142857,0.991071428571429,1.),.UNSPECIFIED.)
GEOMETRIC_REPRESENTATION_ITEM()
RATIONAL_B_SPLINE_SURFACE(((1.,0.923879532511287,1.,0.923879532511287,1.,
0.923879532511287,1.,0.923879532511287,1.,0.923879532511287,1.,0.923879532511287,
1.,0.923879532511287,1.,0.923879532511287,1.,0.923879532511287,1.,0.923879532511287,
1.,0.923879532511287,1.,0.923879532511287,1.,0.923879532511287,1.,0.923879532511287,
1.,0.923879532511287,1.,0.923879532511287,1.,0.923879532511287,1.,0.923879532511287,
1.,0.923879532511287,1.,0.923879532511287,1.,0.923879532511287,1.,0.923879532511287,
1.,0.923879532511287,1.,0.923879532511287,1.,0.923879532511287,1.,0.923879532511287,
1.,0.923879532511287,1.,0.923879532511287,1.,0.923879532511287,1.,0.923879532511287,
1.,0.923879532511287,1.,0.923879532511287,1.,0.923879532511287,1.,0.923879532511287,
1.,0.923879532511287,1.,0.923879532511287,1.,0.923879532511287,1.,0.923879532511287,
1.,0.923879532511287,1.,0.923879532511287,1.,0.923879532511287,1.,0.923879532511287,
1.,0.923879532511287,1.,0.923879532511287,1.,0.923879532511287,1.,0.923879532511287,
1.,0.923879532511287,1.,0.923879532511287,1.,0.923879532511287,1.,0.923879532511287,
1.,0.923879532511287,1.,0.923879532511287,1.,0.923879532511287,1.,0.923879532511287,
1.,0.923879532511287,1.,0.923879532511287,1.,0.923879532511287,1.,0.923879532511287,
1.,0.923879532511287,1.,0.923879532511287,1.,0.923879532511287,1.,0.923879532511287,
1.,0.923879532511287,1.,0.923879532511287,1.,0.923879532511287,1.,0.923879532511287,
1.,0.923879532511287,1.,0.923879532511287,1.,0.923879532511287,1.,0.923879532511287,
1.,0.923879532511287,1.,0.923879532511287,1.,0.923879532511287,1.,0.923879532511287,
1.,0.923879532511287,1.,0.923879532511287,1.,0.923879532511287,1.,0.923879532511287,
1.,0.923879532511287,1.,0.923879532511287,1.,0.923879532511287,1.,0.923879532511287,
1.,0.923879532511287,1.,0.923879532511287,1.,0.923879532511287,1.,0.923879532511287,
1.,0.923879532511287,1.,0.923879532511287,1.,0.923879532511287,1.,0.923879532511287,
1.,0.923879532511287,1.,0.923879532511287,1.,0.923879532511287,1.,0.923879532511287,
1.,0.923879532511287,1.,0.923879532511287,1.,0.923879532511287,1.,0.923879532511287,
1.,0.923879532511287,1.,0.923879532511287,1.,0.923879532511287,1.,0.923879532511287,
1.,0.923879532511287,1.,0.923879532511287,1.,0.923879532511287,1.,0.923879532511287,
1.,0.923879532511287,1.,0.923879532511287,1.,0.923879532511287,1.,0.923879532511287,
1.,0.923879532511287,1.,0.923879532511287,1.),(1.,0.923879532511287,1.,
0.923879532511287,1.,0.923879532511287,1.,0.923879532511287,1.,0.923879532511287,
1.,0.923879532511287,1.,0.923879532511287,1.,0.923879532511287,1.,0.923879532511287,
1.,0.923879532511287,1.,0.923879532511287,1.,0.923879532511287,1.,0.923879532511287,
1.,0.923879532511287,1.,0.923879532511287,1.,0.923879532511287,1.,0.923879532511287,
1.,0.923879532511287,1.,0.923879532511287,1.,0.923879532511287,1.,0.923879532511287,
1.,0.923879532511287,1.,0.923879532511287,1.,0.923879532511287,1.,0.923879532511287,
1.,0.923879532511287,1.,0.923879532511287,1.,0.923879532511287,1.,0.923879532511287,
1.,0.923879532511287,1.,0.923879532511287,1.,0.923879532511287,1.,0.923879532511287,
1.,0.923879532511287,1.,0.923879532511287,1.,0.923879532511287,1.,0.923879532511287,
1.,0.923879532511287,1.,0.923879532511287,1.,0.923879532511287,1.,0.923879532511287,
1.,0.923879532511287,1.,0.923879532511287,1.,0.923879532511287,1.,0.923879532511287,
1.,0.923879532511287,1.,0.923879532511287,1.,0.923879532511287,1.,0.923879532511287,
1.,0.923879532511287,1.,0.923879532511287,1.,0.923879532511287,1.,0.923879532511287,
1.,0.923879532511287,1.,0.923879532511287,1.,0.923879532511287,1.,0.923879532511287,
1.,0.923879532511287,1.,0.923879532511287,1.,0.923879532511287,1.,0.923879532511287,
1.,0.923879532511287,1.,0.923879532511287,1.,0.923879532511287,1.,0.923879532511287,
1.,0.923879532511287,1.,0.923879532511287,1.,0.923879532511287,1.,0.923879532511287,
1.,0.923879532511287,1.,0.923879532511287,1.,0.923879532511287,1.,0.923879532511287,
1.,0.923879532511287,1.,0.923879532511287,1.,0.923879532511287,1.,0.923879532511287,
1.,0.923879532511287,1.,0.923879532511287,1.,0.923879532511287,1.,0.923879532511287,
1.,0.923879532511287,1.,0.923879532511287,1.,0.923879532511287,1.,0.923879532511287,
1.,0.923879532511287,1.,0.923879532511287,1.,0.923879532511287,1.,0.923879532511287,
1.,0.923879532511287,1.,0.923879532511287,1.,0.923879532511287,1.,0.923879532511287,
1.,0.923879532511287,1.,0.923879532511287,1.,0.923879532511287,1.,0.923879532511287,
1.,0.923879532511287,1.,0.923879532511287,1.,0.923879532511287,1.,0.923879532511287,
1.,0.923879532511287,1.,0.923879532511287,1.,0.923879532511287,1.,0.923879532511287,
1.,0.923879532511287,1.,0.923879532511287,1.,0.923879532511287,1.,0.923879532511287,
1.,0.923879532511287,1.,0.923879532511287,1.,0.923879532511287,1.)))
REPRESENTATION_ITEM('')
SURFACE()
);
#325=(
BOUNDED_SURFACE()
B_SPLINE_SURFACE(1,2,((#27042,#27043,#27044,#27045,#27046,#27047,#27048,
#27049,#27050,#27051,#27052,#27053,#27054,#27055,#27056,#27057,#27058,#27059,
#27060,#27061,#27062,#27063,#27064,#27065,#27066,#27067,#27068,#27069,#27070,
#27071,#27072,#27073,#27074,#27075,#27076,#27077,#27078,#27079,#27080,#27081,
#27082,#27083,#27084,#27085,#27086,#27087,#27088,#27089,#27090,#27091,#27092,
#27093,#27094,#27095,#27096,#27097,#27098,#27099,#27100,#27101,#27102,#27103,
#27104,#27105,#27106,#27107,#27108,#27109,#27110,#27111,#27112,#27113,#27114,
#27115,#27116,#27117,#27118,#27119,#27120,#27121,#27122,#27123,#27124,#27125,
#27126,#27127,#27128,#27129,#27130,#27131,#27132,#27133,#27134,#27135,#27136,
#27137,#27138,#27139,#27140,#27141,#27142,#27143,#27144,#27145,#27146,#27147,
#27148,#27149,#27150,#27151,#27152,#27153,#27154,#27155,#27156,#27157,#27158,
#27159,#27160,#27161,#27162,#27163,#27164,#27165,#27166,#27167,#27168,#27169,
#27170,#27171,#27172,#27173,#27174,#27175,#27176,#27177,#27178,#27179,#27180,
#27181,#27182,#27183,#27184,#27185,#27186,#27187,#27188,#27189,#27190,#27191,
#27192,#27193,#27194,#27195,#27196,#27197,#27198,#27199,#27200,#27201,#27202),
(#27203,#27204,#27205,#27206,#27207,#27208,#27209,#27210,#27211,#27212,
#27213,#27214,#27215,#27216,#27217,#27218,#27219,#27220,#27221,#27222,#27223,
#27224,#27225,#27226,#27227,#27228,#27229,#27230,#27231,#27232,#27233,#27234,
#27235,#27236,#27237,#27238,#27239,#27240,#27241,#27242,#27243,#27244,#27245,
#27246,#27247,#27248,#27249,#27250,#27251,#27252,#27253,#27254,#27255,#27256,
#27257,#27258,#27259,#27260,#27261,#27262,#27263,#27264,#27265,#27266,#27267,
#27268,#27269,#27270,#27271,#27272,#27273,#27274,#27275,#27276,#27277,#27278,
#27279,#27280,#27281,#27282,#27283,#27284,#27285,#27286,#27287,#27288,#27289,
#27290,#27291,#27292,#27293,#27294,#27295,#27296,#27297,#27298,#27299,#27300,
#27301,#27302,#27303,#27304,#27305,#27306,#27307,#27308,#27309,#27310,#27311,
#27312,#27313,#27314,#27315,#27316,#27317,#27318,#27319,#27320,#27321,#27322,
#27323,#27324,#27325,#27326,#27327,#27328,#27329,#27330,#27331,#27332,#27333,
#27334,#27335,#27336,#27337,#27338,#27339,#27340,#27341,#27342,#27343,#27344,
#27345,#27346,#27347,#27348,#27349,#27350,#27351,#27352,#27353,#27354,#27355,
#27356,#27357,#27358,#27359,#27360,#27361,#27362,#27363)),.UNSPECIFIED.,
 .F.,.F.,.F.)
B_SPLINE_SURFACE_WITH_KNOTS((2,2),(3,2,2,2,2,2,2,2,2,2,2,2,2,2,2,2,2,2,
2,2,2,2,2,2,2,2,2,2,2,2,2,2,2,2,2,2,2,2,2,2,2,2,2,2,2,2,2,2,2,2,2,2,2,2,
2,2,2,2,2,2,2,2,2,2,2,2,2,2,2,2,2,2,2,2,2,2,2,2,2,2,3),(0.,1.),(0.,0.0125,
0.025,0.0375,0.05,0.0625,0.075,0.0875,0.1,0.1125,0.125,0.1375,0.15,0.1625,
0.175,0.1875,0.2,0.2125,0.225,0.2375,0.25,0.2625,0.275,0.2875,0.3,0.3125,
0.325,0.3375,0.35,0.3625,0.375,0.3875,0.4,0.4125,0.425,0.4375,0.45,0.4625,
0.475,0.4875,0.5,0.5125,0.525,0.5375,0.55,0.5625,0.575,0.5875,0.6,0.6125,
0.625,0.6375,0.65,0.6625,0.675,0.6875,0.7,0.7125,0.725,0.7375,0.75,0.7625,
0.775,0.7875,0.8,0.8125,0.825,0.8375,0.85,0.8625,0.875,0.8875,0.9,0.9125,
0.925,0.9375,0.95,0.9625,0.975,0.9875,1.),.UNSPECIFIED.)
GEOMETRIC_REPRESENTATION_ITEM()
RATIONAL_B_SPLINE_SURFACE(((1.,0.923879532511287,1.,0.923879532511287,1.,
0.923879532511287,1.,0.923879532511287,1.,0.923879532511287,1.,0.923879532511287,
1.,0.923879532511287,1.,0.923879532511287,1.,0.923879532511287,1.,0.923879532511287,
1.,0.923879532511287,1.,0.923879532511287,1.,0.923879532511287,1.,0.923879532511287,
1.,0.923879532511287,1.,0.923879532511287,1.,0.923879532511287,1.,0.923879532511287,
1.,0.923879532511287,1.,0.923879532511287,1.,0.923879532511287,1.,0.923879532511287,
1.,0.923879532511287,1.,0.923879532511287,1.,0.923879532511287,1.,0.923879532511287,
1.,0.923879532511287,1.,0.923879532511287,1.,0.923879532511287,1.,0.923879532511287,
1.,0.923879532511287,1.,0.923879532511287,1.,0.923879532511287,1.,0.923879532511287,
1.,0.923879532511287,1.,0.923879532511287,1.,0.923879532511287,1.,0.923879532511287,
1.,0.923879532511287,1.,0.923879532511287,1.,0.923879532511287,1.,0.923879532511287,
1.,0.923879532511287,1.,0.923879532511287,1.,0.923879532511287,1.,0.923879532511287,
1.,0.923879532511287,1.,0.923879532511287,1.,0.923879532511287,1.,0.923879532511287,
1.,0.923879532511287,1.,0.923879532511287,1.,0.923879532511287,1.,0.923879532511287,
1.,0.923879532511287,1.,0.923879532511287,1.,0.923879532511287,1.,0.923879532511287,
1.,0.923879532511287,1.,0.923879532511287,1.,0.923879532511287,1.,0.923879532511287,
1.,0.923879532511287,1.,0.923879532511287,1.,0.923879532511287,1.,0.923879532511287,
1.,0.923879532511287,1.,0.923879532511287,1.,0.923879532511287,1.,0.923879532511287,
1.,0.923879532511287,1.,0.923879532511287,1.,0.923879532511287,1.,0.923879532511287,
1.,0.923879532511287,1.,0.923879532511287,1.,0.923879532511287,1.,0.923879532511287,
1.,0.923879532511287,1.,0.923879532511287,1.),(1.,0.923879532511287,1.,
0.923879532511287,1.,0.923879532511287,1.,0.923879532511287,1.,0.923879532511287,
1.,0.923879532511287,1.,0.923879532511287,1.,0.923879532511287,1.,0.923879532511287,
1.,0.923879532511287,1.,0.923879532511287,1.,0.923879532511287,1.,0.923879532511287,
1.,0.923879532511287,1.,0.923879532511287,1.,0.923879532511287,1.,0.923879532511287,
1.,0.923879532511287,1.,0.923879532511287,1.,0.923879532511287,1.,0.923879532511287,
1.,0.923879532511287,1.,0.923879532511287,1.,0.923879532511287,1.,0.923879532511287,
1.,0.923879532511287,1.,0.923879532511287,1.,0.923879532511287,1.,0.923879532511287,
1.,0.923879532511287,1.,0.923879532511287,1.,0.923879532511287,1.,0.923879532511287,
1.,0.923879532511287,1.,0.923879532511287,1.,0.923879532511287,1.,0.923879532511287,
1.,0.923879532511287,1.,0.923879532511287,1.,0.923879532511287,1.,0.923879532511287,
1.,0.923879532511287,1.,0.923879532511287,1.,0.923879532511287,1.,0.923879532511287,
1.,0.923879532511287,1.,0.923879532511287,1.,0.923879532511287,1.,0.923879532511287,
1.,0.923879532511287,1.,0.923879532511287,1.,0.923879532511287,1.,0.923879532511287,
1.,0.923879532511287,1.,0.923879532511287,1.,0.923879532511287,1.,0.923879532511287,
1.,0.923879532511287,1.,0.923879532511287,1.,0.923879532511287,1.,0.923879532511287,
1.,0.923879532511287,1.,0.923879532511287,1.,0.923879532511287,1.,0.923879532511287,
1.,0.923879532511287,1.,0.923879532511287,1.,0.923879532511287,1.,0.923879532511287,
1.,0.923879532511287,1.,0.923879532511287,1.,0.923879532511287,1.,0.923879532511287,
1.,0.923879532511287,1.,0.923879532511287,1.,0.923879532511287,1.,0.923879532511287,
1.,0.923879532511287,1.,0.923879532511287,1.,0.923879532511287,1.)))
REPRESENTATION_ITEM('')
SURFACE()
);
#326=(
BOUNDED_SURFACE()
B_SPLINE_SURFACE(1,2,((#27364,#27365,#27366,#27367,#27368,#27369,#27370,
#27371,#27372,#27373,#27374,#27375,#27376,#27377,#27378,#27379,#27380,#27381,
#27382,#27383,#27384,#27385,#27386,#27387,#27388,#27389,#27390,#27391,#27392,
#27393,#27394,#27395,#27396,#27397,#27398,#27399,#27400,#27401,#27402,#27403,
#27404,#27405,#27406,#27407,#27408,#27409,#27410,#27411,#27412,#27413,#27414,
#27415,#27416,#27417,#27418,#27419,#27420,#27421,#27422,#27423,#27424,#27425,
#27426,#27427,#27428,#27429,#27430,#27431,#27432,#27433,#27434,#27435,#27436,
#27437,#27438,#27439,#27440,#27441,#27442,#27443,#27444,#27445,#27446,#27447,
#27448,#27449,#27450,#27451,#27452,#27453,#27454,#27455,#27456,#27457,#27458,
#27459,#27460,#27461,#27462,#27463,#27464,#27465,#27466,#27467,#27468,#27469,
#27470,#27471,#27472,#27473,#27474,#27475,#27476,#27477,#27478,#27479,#27480,
#27481,#27482,#27483,#27484,#27485,#27486,#27487,#27488,#27489,#27490,#27491,
#27492,#27493,#27494,#27495,#27496,#27497,#27498,#27499,#27500,#27501,#27502,
#27503,#27504,#27505,#27506,#27507,#27508,#27509,#27510,#27511,#27512,#27513,
#27514,#27515,#27516,#27517,#27518,#27519,#27520,#27521,#27522,#27523,#27524),
(#27525,#27526,#27527,#27528,#27529,#27530,#27531,#27532,#27533,#27534,
#27535,#27536,#27537,#27538,#27539,#27540,#27541,#27542,#27543,#27544,#27545,
#27546,#27547,#27548,#27549,#27550,#27551,#27552,#27553,#27554,#27555,#27556,
#27557,#27558,#27559,#27560,#27561,#27562,#27563,#27564,#27565,#27566,#27567,
#27568,#27569,#27570,#27571,#27572,#27573,#27574,#27575,#27576,#27577,#27578,
#27579,#27580,#27581,#27582,#27583,#27584,#27585,#27586,#27587,#27588,#27589,
#27590,#27591,#27592,#27593,#27594,#27595,#27596,#27597,#27598,#27599,#27600,
#27601,#27602,#27603,#27604,#27605,#27606,#27607,#27608,#27609,#27610,#27611,
#27612,#27613,#27614,#27615,#27616,#27617,#27618,#27619,#27620,#27621,#27622,
#27623,#27624,#27625,#27626,#27627,#27628,#27629,#27630,#27631,#27632,#27633,
#27634,#27635,#27636,#27637,#27638,#27639,#27640,#27641,#27642,#27643,#27644,
#27645,#27646,#27647,#27648,#27649,#27650,#27651,#27652,#27653,#27654,#27655,
#27656,#27657,#27658,#27659,#27660,#27661,#27662,#27663,#27664,#27665,#27666,
#27667,#27668,#27669,#27670,#27671,#27672,#27673,#27674,#27675,#27676,#27677,
#27678,#27679,#27680,#27681,#27682,#27683,#27684,#27685)),.UNSPECIFIED.,
 .F.,.F.,.F.)
B_SPLINE_SURFACE_WITH_KNOTS((2,2),(3,2,2,2,2,2,2,2,2,2,2,2,2,2,2,2,2,2,
2,2,2,2,2,2,2,2,2,2,2,2,2,2,2,2,2,2,2,2,2,2,2,2,2,2,2,2,2,2,2,2,2,2,2,2,
2,2,2,2,2,2,2,2,2,2,2,2,2,2,2,2,2,2,2,2,2,2,2,2,2,2,3),(0.,1.),(0.,0.0125,
0.025,0.0375,0.05,0.0625,0.075,0.0875,0.1,0.1125,0.125,0.1375,0.15,0.1625,
0.175,0.1875,0.2,0.2125,0.225,0.2375,0.25,0.2625,0.275,0.2875,0.3,0.3125,
0.325,0.3375,0.35,0.3625,0.375,0.3875,0.4,0.4125,0.425,0.4375,0.45,0.4625,
0.475,0.4875,0.5,0.5125,0.525,0.5375,0.55,0.5625,0.575,0.5875,0.6,0.6125,
0.625,0.6375,0.65,0.6625,0.675,0.6875,0.7,0.7125,0.725,0.7375,0.75,0.7625,
0.775,0.7875,0.8,0.8125,0.825,0.8375,0.85,0.8625,0.875,0.8875,0.9,0.9125,
0.925,0.9375,0.95,0.9625,0.975,0.9875,1.),.UNSPECIFIED.)
GEOMETRIC_REPRESENTATION_ITEM()
RATIONAL_B_SPLINE_SURFACE(((1.,0.923879532511287,1.,0.923879532511287,1.,
0.923879532511287,1.,0.923879532511287,1.,0.923879532511287,1.,0.923879532511287,
1.,0.923879532511287,1.,0.923879532511287,1.,0.923879532511287,1.,0.923879532511287,
1.,0.923879532511287,1.,0.923879532511287,1.,0.923879532511287,1.,0.923879532511287,
1.,0.923879532511287,1.,0.923879532511287,1.,0.923879532511287,1.,0.923879532511287,
1.,0.923879532511287,1.,0.923879532511287,1.,0.923879532511287,1.,0.923879532511287,
1.,0.923879532511287,1.,0.923879532511287,1.,0.923879532511287,1.,0.923879532511287,
1.,0.923879532511287,1.,0.923879532511287,1.,0.923879532511287,1.,0.923879532511287,
1.,0.923879532511287,1.,0.923879532511287,1.,0.923879532511287,1.,0.923879532511287,
1.,0.923879532511287,1.,0.923879532511287,1.,0.923879532511287,1.,0.923879532511287,
1.,0.923879532511287,1.,0.923879532511287,1.,0.923879532511287,1.,0.923879532511287,
1.,0.923879532511287,1.,0.923879532511287,1.,0.923879532511287,1.,0.923879532511287,
1.,0.923879532511287,1.,0.923879532511287,1.,0.923879532511287,1.,0.923879532511287,
1.,0.923879532511287,1.,0.923879532511287,1.,0.923879532511287,1.,0.923879532511287,
1.,0.923879532511287,1.,0.923879532511287,1.,0.923879532511287,1.,0.923879532511287,
1.,0.923879532511287,1.,0.923879532511287,1.,0.923879532511287,1.,0.923879532511287,
1.,0.923879532511287,1.,0.923879532511287,1.,0.923879532511287,1.,0.923879532511287,
1.,0.923879532511287,1.,0.923879532511287,1.,0.923879532511287,1.,0.923879532511287,
1.,0.923879532511287,1.,0.923879532511287,1.,0.923879532511287,1.,0.923879532511287,
1.,0.923879532511287,1.,0.923879532511287,1.,0.923879532511287,1.,0.923879532511287,
1.,0.923879532511287,1.,0.923879532511287,1.),(1.,0.923879532511287,1.,
0.923879532511287,1.,0.923879532511287,1.,0.923879532511287,1.,0.923879532511287,
1.,0.923879532511287,1.,0.923879532511287,1.,0.923879532511287,1.,0.923879532511287,
1.,0.923879532511287,1.,0.923879532511287,1.,0.923879532511287,1.,0.923879532511287,
1.,0.923879532511287,1.,0.923879532511287,1.,0.923879532511287,1.,0.923879532511287,
1.,0.923879532511287,1.,0.923879532511287,1.,0.923879532511287,1.,0.923879532511287,
1.,0.923879532511287,1.,0.923879532511287,1.,0.923879532511287,1.,0.923879532511287,
1.,0.923879532511287,1.,0.923879532511287,1.,0.923879532511287,1.,0.923879532511287,
1.,0.923879532511287,1.,0.923879532511287,1.,0.923879532511287,1.,0.923879532511287,
1.,0.923879532511287,1.,0.923879532511287,1.,0.923879532511287,1.,0.923879532511287,
1.,0.923879532511287,1.,0.923879532511287,1.,0.923879532511287,1.,0.923879532511287,
1.,0.923879532511287,1.,0.923879532511287,1.,0.923879532511287,1.,0.923879532511287,
1.,0.923879532511287,1.,0.923879532511287,1.,0.923879532511287,1.,0.923879532511287,
1.,0.923879532511287,1.,0.923879532511287,1.,0.923879532511287,1.,0.923879532511287,
1.,0.923879532511287,1.,0.923879532511287,1.,0.923879532511287,1.,0.923879532511287,
1.,0.923879532511287,1.,0.923879532511287,1.,0.923879532511287,1.,0.923879532511287,
1.,0.923879532511287,1.,0.923879532511287,1.,0.923879532511287,1.,0.923879532511287,
1.,0.923879532511287,1.,0.923879532511287,1.,0.923879532511287,1.,0.923879532511287,
1.,0.923879532511287,1.,0.923879532511287,1.,0.923879532511287,1.,0.923879532511287,
1.,0.923879532511287,1.,0.923879532511287,1.,0.923879532511287,1.,0.923879532511287,
1.,0.923879532511287,1.,0.923879532511287,1.,0.923879532511287,1.)))
REPRESENTATION_ITEM('')
SURFACE()
);
#327=SPHERICAL_SURFACE('',#12617,4.);
#328=SPHERICAL_SURFACE('',#12619,4.);
#329=SPHERICAL_SURFACE('',#12793,42.2295496985778);
#330=SPHERICAL_SURFACE('',#12810,50.);
#331=SPHERICAL_SURFACE('',#13311,1.);
#332=SPHERICAL_SURFACE('',#13315,1.);
#333=SPHERICAL_SURFACE('',#13340,1.);
#334=SPHERICAL_SURFACE('',#13344,1.);
#335=FACE_BOUND('',#2001,.T.);
#336=FACE_BOUND('',#2002,.T.);
#337=FACE_BOUND('',#2003,.T.);
#338=FACE_BOUND('',#2004,.T.);
#339=FACE_BOUND('',#2005,.T.);
#340=FACE_BOUND('',#2007,.T.);
#341=FACE_BOUND('',#2008,.T.);
#342=FACE_BOUND('',#2009,.T.);
#343=FACE_BOUND('',#2014,.T.);
#344=FACE_BOUND('',#2015,.T.);
#345=FACE_BOUND('',#2016,.T.);
#346=FACE_BOUND('',#2017,.T.);
#347=FACE_BOUND('',#2018,.T.);
#348=FACE_BOUND('',#2024,.T.);
#349=FACE_BOUND('',#2029,.T.);
#350=FACE_BOUND('',#2034,.T.);
#351=FACE_BOUND('',#2051,.T.);
#352=FACE_BOUND('',#2053,.T.);
#353=FACE_BOUND('',#2055,.T.);
#354=FACE_BOUND('',#2061,.T.);
#355=FACE_BOUND('',#2062,.T.);
#356=FACE_BOUND('',#2063,.T.);
#357=FACE_BOUND('',#2065,.T.);
#358=FACE_BOUND('',#2067,.T.);
#359=FACE_BOUND('',#2072,.T.);
#360=FACE_BOUND('',#2083,.T.);
#361=FACE_BOUND('',#2085,.T.);
#362=FACE_BOUND('',#2087,.T.);
#363=FACE_BOUND('',#2137,.T.);
#364=FACE_BOUND('',#2138,.T.);
#365=FACE_BOUND('',#2142,.T.);
#366=FACE_BOUND('',#2143,.T.);
#367=FACE_BOUND('',#2144,.T.);
#368=FACE_BOUND('',#2152,.T.);
#369=FACE_BOUND('',#2153,.T.);
#370=FACE_BOUND('',#2178,.T.);
#371=FACE_BOUND('',#2179,.T.);
#372=FACE_BOUND('',#2180,.T.);
#373=FACE_BOUND('',#2182,.T.);
#374=FACE_BOUND('',#2184,.T.);
#375=FACE_BOUND('',#2200,.T.);
#376=FACE_BOUND('',#2209,.T.);
#377=FACE_BOUND('',#2215,.T.);
#378=FACE_BOUND('',#2260,.T.);
#379=FACE_BOUND('',#2261,.T.);
#380=FACE_BOUND('',#2263,.T.);
#381=FACE_BOUND('',#2264,.T.);
#382=FACE_BOUND('',#2266,.T.);
#383=FACE_BOUND('',#2268,.T.);
#384=FACE_BOUND('',#2272,.T.);
#385=FACE_BOUND('',#2276,.T.);
#386=FACE_BOUND('',#2278,.T.);
#387=FACE_BOUND('',#2279,.T.);
#388=FACE_BOUND('',#2281,.T.);
#389=FACE_BOUND('',#2282,.T.);
#390=FACE_BOUND('',#2284,.T.);
#391=FACE_BOUND('',#2289,.T.);
#392=FACE_BOUND('',#2291,.T.);
#393=FACE_BOUND('',#2309,.T.);
#394=FACE_BOUND('',#2310,.T.);
#395=FACE_BOUND('',#2312,.T.);
#396=FACE_BOUND('',#2313,.T.);
#397=FACE_BOUND('',#2327,.T.);
#398=FACE_BOUND('',#2341,.T.);
#399=FACE_BOUND('',#2345,.T.);
#400=FACE_BOUND('',#2347,.T.);
#401=FACE_BOUND('',#2351,.T.);
#402=FACE_BOUND('',#2353,.T.);
#403=FACE_BOUND('',#2355,.T.);
#404=FACE_BOUND('',#2357,.T.);
#405=FACE_BOUND('',#2365,.T.);
#406=FACE_BOUND('',#2369,.T.);
#407=FACE_BOUND('',#2371,.T.);
#408=FACE_BOUND('',#2390,.T.);
#409=FACE_BOUND('',#2405,.T.);
#410=FACE_BOUND('',#2443,.T.);
#411=FACE_BOUND('',#2445,.T.);
#412=FACE_BOUND('',#2447,.T.);
#413=FACE_BOUND('',#2449,.T.);
#414=FACE_BOUND('',#2492,.T.);
#415=FACE_BOUND('',#2506,.T.);
#416=FACE_BOUND('',#2542,.T.);
#417=FACE_BOUND('',#2548,.T.);
#418=FACE_BOUND('',#2549,.T.);
#419=FACE_BOUND('',#2551,.T.);
#420=FACE_BOUND('',#2552,.T.);
#421=FACE_BOUND('',#2558,.T.);
#422=FACE_BOUND('',#2559,.T.);
#423=FACE_BOUND('',#2561,.T.);
#424=FACE_BOUND('',#2562,.T.);
#425=FACE_BOUND('',#2573,.T.);
#426=FACE_BOUND('',#2580,.T.);
#427=FACE_BOUND('',#2600,.T.);
#428=FACE_BOUND('',#2602,.T.);
#429=FACE_BOUND('',#2604,.T.);
#430=FACE_BOUND('',#2606,.T.);
#431=FACE_BOUND('',#2608,.T.);
#432=FACE_BOUND('',#2610,.T.);
#433=FACE_BOUND('',#2624,.T.);
#434=FACE_BOUND('',#2626,.T.);
#435=FACE_BOUND('',#2628,.T.);
#436=FACE_BOUND('',#2630,.T.);
#437=FACE_BOUND('',#2632,.T.);
#438=FACE_BOUND('',#2634,.T.);
#439=FACE_BOUND('',#2673,.T.);
#440=FACE_BOUND('',#2675,.T.);
#441=FACE_BOUND('',#2678,.T.);
#442=FACE_BOUND('',#2680,.T.);
#443=FACE_BOUND('',#2691,.T.);
#444=FACE_BOUND('',#2720,.T.);
#445=FACE_BOUND('',#2722,.T.);
#446=FACE_BOUND('',#2724,.T.);
#447=FACE_BOUND('',#2748,.T.);
#448=PLANE('',#12425);
#449=PLANE('',#12427);
#450=PLANE('',#12428);
#451=PLANE('',#12429);
#452=PLANE('',#12431);
#453=PLANE('',#12432);
#454=PLANE('',#12440);
#455=PLANE('',#12443);
#456=PLANE('',#12444);
#457=PLANE('',#12451);
#458=PLANE('',#12452);
#459=PLANE('',#12453);
#460=PLANE('',#12455);
#461=PLANE('',#12457);
#462=PLANE('',#12466);
#463=PLANE('',#12477);
#464=PLANE('',#12478);
#465=PLANE('',#12482);
#466=PLANE('',#12493);
#467=PLANE('',#12494);
#468=PLANE('',#12495);
#469=PLANE('',#12496);
#470=PLANE('',#12497);
#471=PLANE('',#12498);
#472=PLANE('',#12503);
#473=PLANE('',#12506);
#474=PLANE('',#12508);
#475=PLANE('',#12511);
#476=PLANE('',#12513);
#477=PLANE('',#12515);
#478=PLANE('',#12519);
#479=PLANE('',#12521);
#480=PLANE('',#12529);
#481=PLANE('',#12530);
#482=PLANE('',#12533);
#483=PLANE('',#12535);
#484=PLANE('',#12537);
#485=PLANE('',#12540);
#486=PLANE('',#12543);
#487=PLANE('',#12544);
#488=PLANE('',#12545);
#489=PLANE('',#12546);
#490=PLANE('',#12547);
#491=PLANE('',#12548);
#492=PLANE('',#12549);
#493=PLANE('',#12550);
#494=PLANE('',#12558);
#495=PLANE('',#12559);
#496=PLANE('',#12560);
#497=PLANE('',#12562);
#498=PLANE('',#12564);
#499=PLANE('',#12566);
#500=PLANE('',#12571);
#501=PLANE('',#12573);
#502=PLANE('',#12576);
#503=PLANE('',#12577);
#504=PLANE('',#12579);
#505=PLANE('',#12582);
#506=PLANE('',#12583);
#507=PLANE('',#12584);
#508=PLANE('',#12585);
#509=PLANE('',#12588);
#510=PLANE('',#12589);
#511=PLANE('',#12591);
#512=PLANE('',#12592);
#513=PLANE('',#12597);
#514=PLANE('',#12657);
#515=PLANE('',#12665);
#516=PLANE('',#12669);
#517=PLANE('',#12678);
#518=PLANE('',#12681);
#519=PLANE('',#12684);
#520=PLANE('',#12685);
#521=PLANE('',#12686);
#522=PLANE('',#12693);
#523=PLANE('',#12721);
#524=PLANE('',#12726);
#525=PLANE('',#12727);
#526=PLANE('',#12728);
#527=PLANE('',#12729);
#528=PLANE('',#12730);
#529=PLANE('',#12731);
#530=PLANE('',#12732);
#531=PLANE('',#12733);
#532=PLANE('',#12735);
#533=PLANE('',#12736);
#534=PLANE('',#12739);
#535=PLANE('',#12742);
#536=PLANE('',#12763);
#537=PLANE('',#12764);
#538=PLANE('',#12765);
#539=PLANE('',#12779);
#540=PLANE('',#12780);
#541=PLANE('',#12781);
#542=PLANE('',#12834);
#543=PLANE('',#12837);
#544=PLANE('',#12839);
#545=PLANE('',#12840);
#546=PLANE('',#12841);
#547=PLANE('',#12842);
#548=PLANE('',#12843);
#549=PLANE('',#12845);
#550=PLANE('',#12846);
#551=PLANE('',#12847);
#552=PLANE('',#12848);
#553=PLANE('',#12849);
#554=PLANE('',#12850);
#555=PLANE('',#12852);
#556=PLANE('',#12853);
#557=PLANE('',#12854);
#558=PLANE('',#12855);
#559=PLANE('',#12904);
#560=PLANE('',#12908);
#561=PLANE('',#12909);
#562=PLANE('',#12910);
#563=PLANE('',#12913);
#564=PLANE('',#12916);
#565=PLANE('',#12917);
#566=PLANE('',#12920);
#567=PLANE('',#12921);
#568=PLANE('',#12922);
#569=PLANE('',#12927);
#570=PLANE('',#12928);
#571=PLANE('',#12931);
#572=PLANE('',#12934);
#573=PLANE('',#12935);
#574=PLANE('',#12936);
#575=PLANE('',#12937);
#576=PLANE('',#12938);
#577=PLANE('',#12939);
#578=PLANE('',#12953);
#579=PLANE('',#12954);
#580=PLANE('',#12963);
#581=PLANE('',#12964);
#582=PLANE('',#12975);
#583=PLANE('',#12980);
#584=PLANE('',#12985);
#585=PLANE('',#12986);
#586=PLANE('',#12987);
#587=PLANE('',#12988);
#588=PLANE('',#13064);
#589=PLANE('',#13066);
#590=PLANE('',#13067);
#591=PLANE('',#13068);
#592=PLANE('',#13069);
#593=PLANE('',#13072);
#594=PLANE('',#13075);
#595=PLANE('',#13076);
#596=PLANE('',#13077);
#597=PLANE('',#13078);
#598=PLANE('',#13079);
#599=PLANE('',#13080);
#600=PLANE('',#13081);
#601=PLANE('',#13082);
#602=PLANE('',#13083);
#603=PLANE('',#13084);
#604=PLANE('',#13085);
#605=PLANE('',#13086);
#606=PLANE('',#13087);
#607=PLANE('',#13088);
#608=PLANE('',#13089);
#609=PLANE('',#13090);
#610=PLANE('',#13091);
#611=PLANE('',#13093);
#612=PLANE('',#13094);
#613=PLANE('',#13096);
#614=PLANE('',#13097);
#615=PLANE('',#13098);
#616=PLANE('',#13099);
#617=PLANE('',#13100);
#618=PLANE('',#13101);
#619=PLANE('',#13102);
#620=PLANE('',#13103);
#621=PLANE('',#13105);
#622=PLANE('',#13107);
#623=PLANE('',#13110);
#624=PLANE('',#13112);
#625=PLANE('',#13114);
#626=PLANE('',#13117);
#627=PLANE('',#13122);
#628=PLANE('',#13123);
#629=PLANE('',#13124);
#630=PLANE('',#13125);
#631=PLANE('',#13126);
#632=PLANE('',#13127);
#633=PLANE('',#13136);
#634=PLANE('',#13137);
#635=PLANE('',#13182);
#636=PLANE('',#13183);
#637=PLANE('',#13184);
#638=PLANE('',#13185);
#639=PLANE('',#13202);
#640=PLANE('',#13203);
#641=PLANE('',#13204);
#642=PLANE('',#13205);
#643=PLANE('',#13206);
#644=PLANE('',#13207);
#645=PLANE('',#13213);
#646=PLANE('',#13215);
#647=PLANE('',#13217);
#648=PLANE('',#13226);
#649=PLANE('',#13236);
#650=PLANE('',#13238);
#651=PLANE('',#13240);
#652=PLANE('',#13242);
#653=PLANE('',#13245);
#654=PLANE('',#13247);
#655=PLANE('',#13249);
#656=PLANE('',#13251);
#657=PLANE('',#13253);
#658=PLANE('',#13255);
#659=PLANE('',#13256);
#660=PLANE('',#13258);
#661=PLANE('',#13259);
#662=PLANE('',#13260);
#663=PLANE('',#13261);
#664=PLANE('',#13262);
#665=PLANE('',#13280);
#666=PLANE('',#13281);
#667=PLANE('',#13282);
#668=PLANE('',#13299);
#669=PLANE('',#13300);
#670=PLANE('',#13301);
#671=PLANE('',#13398);
#672=PLANE('',#13399);
#673=PLANE('',#13400);
#674=PLANE('',#13401);
#675=PLANE('',#13402);
#676=PLANE('',#13403);
#677=PLANE('',#13404);
#678=PLANE('',#13405);
#679=PLANE('',#13406);
#680=PLANE('',#13407);
#681=PLANE('',#13408);
#682=PLANE('',#13409);
#683=PLANE('',#13410);
#684=PLANE('',#13411);
#685=PLANE('',#13412);
#686=PLANE('',#13413);
#687=PLANE('',#13419);
#688=PLANE('',#13420);
#689=PLANE('',#13433);
#690=PLANE('',#13449);
#691=PLANE('',#13450);
#692=PLANE('',#13451);
#693=PLANE('',#13465);
#694=PLANE('',#13466);
#695=PLANE('',#13506);
#696=PLANE('',#13507);
#697=PLANE('',#13508);
#698=PLANE('',#13509);
#699=PLANE('',#13510);
#700=PLANE('',#13511);
#701=PLANE('',#13554);
#702=PLANE('',#13555);
#703=PLANE('',#13556);
#704=PLANE('',#13557);
#705=PLANE('',#13558);
#706=PLANE('',#13559);
#707=PLANE('',#13568);
#708=PLANE('',#13569);
#709=PLANE('',#13613);
#710=PLANE('',#13614);
#711=PLANE('',#13615);
#712=PLANE('',#13617);
#713=PLANE('',#13619);
#714=PLANE('',#13620);
#715=PLANE('',#13622);
#716=PLANE('',#13624);
#717=PLANE('',#13625);
#718=PLANE('',#13628);
#719=PLANE('',#13631);
#720=PLANE('',#13634);
#721=PLANE('',#13639);
#722=PLANE('',#13642);
#723=PLANE('',#13645);
#724=PLANE('',#13646);
#725=PLANE('',#13647);
#726=PLANE('',#13676);
#727=PLANE('',#13677);
#728=PLANE('',#13678);
#729=PLANE('',#13679);
#730=PLANE('',#13680);
#731=PLANE('',#13681);
#732=PLANE('',#13682);
#733=PLANE('',#13683);
#734=PLANE('',#13684);
#735=PLANE('',#13685);
#736=PLANE('',#13687);
#737=PLANE('',#13688);
#738=PLANE('',#13689);
#739=PLANE('',#13690);
#740=PLANE('',#13691);
#741=PLANE('',#13692);
#742=PLANE('',#13705);
#743=PLANE('',#13706);
#744=PLANE('',#13707);
#745=PLANE('',#13717);
#746=PLANE('',#13718);
#747=ELLIPSE('',#12376,5.6568542494854,3.99999999999488);
#748=ELLIPSE('',#12390,28.164698545175,26.9999999999996);
#749=ELLIPSE('',#12421,31.2941094946442,30.0000000000042);
#750=ELLIPSE('',#12435,141.421352252718,99.9999944851797);
#751=ELLIPSE('',#12449,10.0848897519878,9.99999999999638);
#752=ELLIPSE('',#12450,10.0848897519895,9.99999999999823);
#753=ELLIPSE('',#12456,2.01697795039841,2.0000000000002);
#754=ELLIPSE('',#12465,6.05093385119014,5.9999999999955);
#755=ELLIPSE('',#12492,6.05093385118888,5.99999999999402);
#756=ELLIPSE('',#12502,31.2941094946394,29.9999999999999);
#757=ELLIPSE('',#12504,10.0848897519875,9.99999999999656);
#758=ELLIPSE('',#12505,2.01697795039468,1.99999999999602);
#759=ELLIPSE('',#12510,10.084889751988,9.99999999999652);
#760=ELLIPSE('',#12512,28.1646985451758,27.);
#761=ELLIPSE('',#12520,2.01697795039476,1.99999999999607);
#762=ELLIPSE('',#12523,141.421350791142,99.9999924642367);
#763=ELLIPSE('',#12534,2.82842712474556,1.9999999999995);
#764=ELLIPSE('',#12538,2.8284271247638,2.00000000001808);
#765=ELLIPSE('',#12539,6.36396103068019,4.50000000000073);
#766=ELLIPSE('',#12561,4.00607672981957,4.00312101599644);
#767=ELLIPSE('',#12565,2.01697795039961,2.00000000000168);
#768=ELLIPSE('',#12574,6.36396103067894,4.49999999999996);
#769=ELLIPSE('',#12575,2.82842712478915,2.00000000005605);
#770=ELLIPSE('',#12578,2.82842712474301,1.99999999999741);
#771=ELLIPSE('',#12607,5.65685424949513,4.00000000000238);
#772=ELLIPSE('',#13020,15.2752523147936,9.99999999941178);
#773=ELLIPSE('',#13021,26.5583854086538,10.0763972703331);
#774=ELLIPSE('',#13022,15.2752523156182,9.99999999956869);
#775=ELLIPSE('',#13023,15.2752523175753,10.0000000004984);
#776=ELLIPSE('',#13024,26.4596124709186,10.0015871705796);
#777=ELLIPSE('',#13026,15.2752523173838,10.0000000004154);
#778=ELLIPSE('',#13027,15.2752523164649,9.99999999997215);
#779=ELLIPSE('',#13028,26.5080625328222,10.0382481169211);
#780=ELLIPSE('',#13029,15.2752523159837,9.99999999981764);
#781=ELLIPSE('',#13030,26.3957862331476,9.95339341267837);
#782=ELLIPSE('',#13057,24.57405701212,24.4042521334787);
#783=ELLIPSE('',#13104,15.2752523161817,9.99999999983578);
#784=ELLIPSE('',#13106,15.2752523172107,10.0000000003347);
#785=ELLIPSE('',#13108,15.2752523165152,9.99999999997849);
#786=ELLIPSE('',#13109,15.275252318401,10.0000000008983);
#787=ELLIPSE('',#13111,15.2752523172003,10.0000000003286);
#788=ELLIPSE('',#13113,15.2752523153524,9.99999999942849);
#789=ELLIPSE('',#13115,15.2752523169171,10.0000000001759);
#790=ELLIPSE('',#13116,15.2752523156397,9.99999999956927);
#791=ELLIPSE('',#13118,15.275252316396,9.99999999996106);
#792=ELLIPSE('',#13119,15.2752523165357,10.0000000000049);
#793=ELLIPSE('',#13120,15.2752523165945,10.0000000000236);
#794=ELLIPSE('',#13121,15.2752523165696,10.0000000000157);
#795=ELLIPSE('',#13129,26.271953617607,9.86022278604482);
#796=ELLIPSE('',#13132,26.3549599721588,9.92262765998257);
#797=ELLIPSE('',#13152,1.15470053837393,0.999999999995315);
#798=ELLIPSE('',#13153,1.15470053837848,0.999999999999286);
#799=ELLIPSE('',#13155,1.15470053838003,1.00000000000053);
#800=ELLIPSE('',#13157,1.15470053838039,1.00000000000101);
#801=ELLIPSE('',#13159,1.15470053837954,1.00000000000047);
#802=ELLIPSE('',#13161,1.15470053838034,1.00000000000108);
#803=ELLIPSE('',#13632,5.35545030114693,4.99999999989344);
#804=ELLIPSE('',#13633,2.14218012048347,1.99999999999931);
#805=ELLIPSE('',#13635,5.00338652687943,4.99999999999998);
#806=ELLIPSE('',#13636,2.00135461075165,1.99999999999923);
#807=ELLIPSE('',#13640,5.00338652687943,4.99999999999998);
#808=ELLIPSE('',#13641,2.0013546107478,1.99999999999585);
#809=ELLIPSE('',#13643,5.3554503002225,4.99999999823902);
#810=ELLIPSE('',#13644,2.14218012048814,2.00000000000341);
#811=TOROIDAL_SURFACE('',#12321,24.,6.);
#812=TOROIDAL_SURFACE('',#12326,18.,2.);
#813=TOROIDAL_SURFACE('',#12330,15.,2.);
#814=TOROIDAL_SURFACE('',#12334,15.,2.);
#815=TOROIDAL_SURFACE('',#12338,18.,2.);
#816=TOROIDAL_SURFACE('',#12342,15.,2.);
#817=TOROIDAL_SURFACE('',#12348,15.,2.);
#818=TOROIDAL_SURFACE('',#12354,11.5,2.);
#819=TOROIDAL_SURFACE('',#12359,11.5,2.);
#820=TOROIDAL_SURFACE('',#12363,11.5,2.);
#821=TOROIDAL_SURFACE('',#12368,11.5,2.);
#822=TOROIDAL_SURFACE('',#12378,23.,4.);
#823=TOROIDAL_SURFACE('',#12625,23.,4.);
#824=TOROIDAL_SURFACE('',#12640,24.,6.);
#825=TOROIDAL_SURFACE('',#12701,17.,2.);
#826=TOROIDAL_SURFACE('',#12704,17.,2.);
#827=TOROIDAL_SURFACE('',#12863,15.,2.);
#828=TOROIDAL_SURFACE('',#12868,15.,2.);
#829=TOROIDAL_SURFACE('',#12997,11.5,2.);
#830=TOROIDAL_SURFACE('',#13002,11.5,2.);
#831=TOROIDAL_SURFACE('',#13209,3.95,0.925000000000001);
#832=TOROIDAL_SURFACE('',#13271,4.59999999999999,0.6);
#833=TOROIDAL_SURFACE('',#13290,4.59999999999999,0.6);
#834=TOROIDAL_SURFACE('',#13303,5.00000000000001,1.);
#835=TOROIDAL_SURFACE('',#13307,5.,1.);
#836=TOROIDAL_SURFACE('',#13332,5.00000000000001,1.);
#837=TOROIDAL_SURFACE('',#13336,5.,1.);
#838=TOROIDAL_SURFACE('',#13421,10.,2.);
#839=TOROIDAL_SURFACE('',#13423,12.,2.);
#840=TOROIDAL_SURFACE('',#13435,22.,2.);
#841=TOROIDAL_SURFACE('',#13440,22.,2.);
#842=TOROIDAL_SURFACE('',#13475,23.,2.);
#843=TOROIDAL_SURFACE('',#13480,18.,2.);
#844=TOROIDAL_SURFACE('',#13484,23.,2.);
#845=TOROIDAL_SURFACE('',#13489,18.,2.);
#846=TOROIDAL_SURFACE('',#13523,23.,2.);
#847=TOROIDAL_SURFACE('',#13528,18.,2.);
#848=TOROIDAL_SURFACE('',#13532,23.,2.);
#849=TOROIDAL_SURFACE('',#13537,18.,2.);
#850=B_SPLINE_CURVE_WITH_KNOTS('',3,(#17467,#17468,#17469,#17470,#17471,
#17472,#17473,#17474,#17475,#17476,#17477,#17478),.UNSPECIFIED.,.F.,.F.,
(4,2,2,2,2,4),(2.0099992972745,2.20224824152656,2.28793503314165,2.37362182475674,
2.53832634192652,2.7030308590963),.UNSPECIFIED.);
#851=B_SPLINE_CURVE_WITH_KNOTS('',3,(#17597,#17598,#17599,#17600,#17601,
#17602,#17603,#17604,#17605,#17606,#17607,#17608),.UNSPECIFIED.,.F.,.F.,
(4,2,2,2,2,4),(0.,0.00181440406025865,0.00272160609038796,0.00362880812051727,
0.00544321218077591,0.00725761624103455),.UNSPECIFIED.);
#852=B_SPLINE_CURVE_WITH_KNOTS('',3,(#17643,#17644,#17645,#17646,#17647,
#17648,#17649,#17650,#17651,#17652,#17653,#17654),.UNSPECIFIED.,.F.,.F.,
(4,2,2,2,2,4),(0.,0.00181440406025865,0.00272160609038798,0.0036288081205173,
0.00544321218077593,0.00725761624103456),.UNSPECIFIED.);
#853=B_SPLINE_CURVE_WITH_KNOTS('',3,(#17772,#17773,#17774,#17775,#17776,
#17777),.UNSPECIFIED.,.F.,.F.,(4,2,4),(-1.89448158063908,-0.947240790319523,
-0.943407967638861),.UNSPECIFIED.);
#854=B_SPLINE_CURVE_WITH_KNOTS('',3,(#18063,#18064,#18065,#18066,#18067,
#18068),.UNSPECIFIED.,.F.,.F.,(4,2,4),(-4.54637383394205,-4.54254101126139,
-3.59530022094183),.UNSPECIFIED.);
#855=B_SPLINE_CURVE_WITH_KNOTS('',3,(#18285,#18286,#18287,#18288,#18289,
#18290,#18291,#18292,#18293,#18294),.UNSPECIFIED.,.F.,.F.,(4,2,2,2,4),(-1.65528023567133,
-1.60355895330957,-1.50636781568743,-1.40917667806529,-1.31726787147769),
 .UNSPECIFIED.);
#856=B_SPLINE_CURVE_WITH_KNOTS('',3,(#18296,#18297,#18298,#18299,#18300,
#18301,#18302,#18303,#18304,#18305),.UNSPECIFIED.,.F.,.F.,(4,2,2,2,4),(-0.723638776454986,
-0.631729969867392,-0.53453883224525,-0.437347694623109,-0.385626412261347),
 .UNSPECIFIED.);
#857=B_SPLINE_CURVE_WITH_KNOTS('',3,(#18306,#18307,#18308,#18309,#18310,
#18311,#18312,#18313,#18314,#18315,#18316,#18317),.UNSPECIFIED.,.F.,.F.,
(4,2,2,2,2,4),(0.207978724543637,0.400227668795699,0.48591446041079,0.57160125202588,
0.736305769195657,0.901010286365433),.UNSPECIFIED.);
#858=B_SPLINE_CURVE_WITH_KNOTS('',3,(#18319,#18320,#18321,#18322,#18323,
#18324,#18325,#18326),.UNSPECIFIED.,.F.,.F.,(4,2,2,4),(0.724350563126704,
0.774624716441459,0.824898869756215,0.828883959825179),.UNSPECIFIED.);
#859=B_SPLINE_CURVE_WITH_KNOTS('',3,(#18327,#18328,#18329,#18330,#18331,
#18332,#18333,#18334),.UNSPECIFIED.,.F.,.F.,(4,2,2,4),(1.23194128218264,
1.2359263722516,1.28620052556636,1.33647467888111),.UNSPECIFIED.);
#860=B_SPLINE_CURVE_WITH_KNOTS('',3,(#18336,#18337,#18338,#18339,#18340,
#18341,#18342,#18343),.UNSPECIFIED.,.F.,.F.,(4,2,2,4),(-0.306062057877202,
-0.255787904562446,-0.205513751247691,-0.201528661178732),.UNSPECIFIED.);
#861=B_SPLINE_CURVE_WITH_KNOTS('',3,(#18344,#18345,#18346,#18347,#18348,
#18349,#18350,#18351),.UNSPECIFIED.,.F.,.F.,(4,2,2,4),(0.201528661178729,
0.205513751247691,0.255787904562446,0.306062057877201),.UNSPECIFIED.);
#862=B_SPLINE_CURVE_WITH_KNOTS('',3,(#18438,#18439,#18440,#18441,#18442,
#18443),.UNSPECIFIED.,.F.,.F.,(4,2,4),(-0.302135903177322,-0.22673410522417,
-0.201580663771353),.UNSPECIFIED.);
#863=B_SPLINE_CURVE_WITH_KNOTS('',3,(#18445,#18446,#18447,#18448,#18449,
#18450),.UNSPECIFIED.,.F.,.F.,(4,2,4),(-0.409607477693974,-0.384454036241157,
-0.309052238288002),.UNSPECIFIED.);
#864=B_SPLINE_CURVE_WITH_KNOTS('',3,(#18452,#18453,#18454,#18455,#18456,
#18457),.UNSPECIFIED.,.F.,.F.,(4,2,4),(-0.302135903177326,-0.226734105224171,
-0.201580663771353),.UNSPECIFIED.);
#865=B_SPLINE_CURVE_WITH_KNOTS('',3,(#18459,#18460,#18461,#18462,#18463,
#18464),.UNSPECIFIED.,.F.,.F.,(4,2,4),(-0.409607477693974,-0.384454036241154,
-0.309052238288002),.UNSPECIFIED.);
#866=B_SPLINE_CURVE_WITH_KNOTS('',3,(#18580,#18581,#18582,#18583,#18584,
#18585,#18586,#18587),.UNSPECIFIED.,.F.,.F.,(4,2,2,4),(1.64653183621645,
1.82629619953337,2.00606056285029,2.42476187739513),.UNSPECIFIED.);
#867=B_SPLINE_CURVE_WITH_KNOTS('',3,(#18614,#18615,#18616,#18617),
 .UNSPECIFIED.,.F.,.F.,(4,4),(0.,0.783684993176865),.UNSPECIFIED.);
#868=B_SPLINE_CURVE_WITH_KNOTS('',3,(#18636,#18637,#18638,#18639),
 .UNSPECIFIED.,.F.,.F.,(4,4),(-2.42476187739513,-1.64107688421826),
 .UNSPECIFIED.);
#869=B_SPLINE_CURVE_WITH_KNOTS('',3,(#18646,#18647,#18648,#18649,#18650,
#18651,#18652,#18653),.UNSPECIFIED.,.F.,.F.,(4,2,2,4),(-0.778230041178668,
-0.598465677861747,-0.418701314544826,0.),.UNSPECIFIED.);
#870=B_SPLINE_CURVE_WITH_KNOTS('',3,(#18695,#18696,#18697,#18698,#18699,
#18700,#18701,#18702),.UNSPECIFIED.,.F.,.F.,(4,2,2,4),(3.68263908945476,
4.12349601732247,4.56435294519017,5.44606680092558),.UNSPECIFIED.);
#871=B_SPLINE_CURVE_WITH_KNOTS('',3,(#18705,#18706,#18707,#18708,#18709,
#18710,#18711,#18712,#18713,#18714),.UNSPECIFIED.,.F.,.F.,(4,2,2,2,4),(0.,
0.473183086940068,0.946366173880136,1.33890283846488,1.73143950304963),
 .UNSPECIFIED.);
#872=B_SPLINE_CURVE_WITH_KNOTS('',3,(#18725,#18726,#18727,#18728,#18729,
#18730,#18731,#18732,#18733,#18734),.UNSPECIFIED.,.F.,.F.,(4,2,2,2,4),(0.,
0.287218434472245,0.57443686894449,0.807390418400316,1.04034396785614),
 .UNSPECIFIED.);
#873=B_SPLINE_CURVE_WITH_KNOTS('',3,(#18741,#18742,#18743,#18744,#18745,
#18746,#18747,#18748,#18749,#18750),.UNSPECIFIED.,.F.,.F.,(4,2,2,2,4),(2.56810417568796,
2.77815458546554,2.98820499524312,3.29809009872942,3.60797520221572),
 .UNSPECIFIED.);
#874=B_SPLINE_CURVE_WITH_KNOTS('',3,(#19078,#19079,#19080,#19081,#19082,
#19083,#19084,#19085,#19086,#19087,#19088,#19089,#19090,#19091),
 .UNSPECIFIED.,.F.,.F.,(4,2,2,2,2,2,4),(2.17202184366925,2.28922044415962,
2.56626725236737,3.12036086878288,3.67445448519838,3.95150129340613,4.06869989389652),
 .UNSPECIFIED.);
#875=B_SPLINE_CURVE_WITH_KNOTS('',3,(#19095,#19096,#19097,#19098,#19099,
#19100,#19101,#19102),.UNSPECIFIED.,.F.,.F.,(4,2,2,4),(-0.94833902511363,
-0.831140424623256,-0.554093616415504,0.),.UNSPECIFIED.);
#876=B_SPLINE_CURVE_WITH_KNOTS('',3,(#19107,#19108,#19109,#19110,#19111,
#19112,#19113,#19114),.UNSPECIFIED.,.F.,.F.,(4,2,2,4),(0.,0.554093616415503,
0.831140424623253,0.948339025113634),.UNSPECIFIED.);
#877=B_SPLINE_CURVE_WITH_KNOTS('',3,(#19403,#19404,#19405,#19406,#19407,
#19408,#19409,#19410,#19411,#19412,#19413,#19414,#19415,#19416,#19417,#19418,
#19419,#19420),.UNSPECIFIED.,.F.,.F.,(4,2,2,2,2,2,2,2,4),(0.,0.0192470604937845,
0.0384941209875689,0.0593135836604684,0.0801330463333679,0.101727899817301,
0.123322753301234,0.143135709957287,0.162948666613339),.UNSPECIFIED.);
#878=B_SPLINE_CURVE_WITH_KNOTS('',3,(#19424,#19425,#19426,#19427,#19428,
#19429,#19430,#19431,#19432,#19433,#19434,#19435,#19436,#19437,#19438,#19439,
#19440,#19441),.UNSPECIFIED.,.F.,.F.,(4,2,2,2,2,2,2,2,4),(0.162948666613339,
0.181777764507504,0.200606862401668,0.223173739729446,0.245740617057224,
0.267140699938747,0.288540782820269,0.307205908233542,0.325871033646814),
 .UNSPECIFIED.);
#879=B_SPLINE_CURVE_WITH_KNOTS('',3,(#19583,#19584,#19585,#19586),
 .UNSPECIFIED.,.F.,.F.,(4,4),(2.02557768100327E-7,0.0192787307131084),
 .UNSPECIFIED.);
#880=B_SPLINE_CURVE_WITH_KNOTS('',3,(#19591,#19592,#19593,#19594,#19595,
#19596,#19597,#19598,#19599,#19600,#19601,#19602,#19603,#19604,#19605,#19606,
#19607,#19608,#19609,#19610,#19611,#19612),.UNSPECIFIED.,.F.,.F.,(4,3,3,
3,3,3,3,4),(0.0122741017871804,0.0127193579255126,0.013344159318982,0.013690125400826,
0.0139452191691552,0.0145554803714893,0.0151726535547874,0.0156163365512983),
 .UNSPECIFIED.);
#881=B_SPLINE_CURVE_WITH_KNOTS('',3,(#19614,#19615,#19616,#19617,#19618,
#19619,#19620,#19621,#19622,#19623,#19624,#19625,#19626,#19627,#19628,#19629,
#19630,#19631,#19632,#19633,#19634,#19635,#19636,#19637,#19638,#19639,#19640,
#19641,#19642,#19643,#19644,#19645,#19646,#19647,#19648,#19649,#19650,#19651,
#19652,#19653,#19654,#19655,#19656,#19657,#19658,#19659,#19660,#19661,#19662,
#19663,#19664,#19665,#19666,#19667,#19668,#19669,#19670,#19671,#19672,#19673,
#19674,#19675,#19676,#19677,#19678,#19679,#19680),.UNSPECIFIED.,.F.,.F.,
(4,3,3,3,3,3,3,3,3,3,3,3,3,3,3,3,3,3,3,3,3,3,4),(1.38777878078145E-17,0.000359541750743833,
0.000720760360395833,0.000925988989824252,0.00128781683880211,0.00166392003251687,
0.00177264338187088,0.00185197797964849,0.00229111858557702,0.00274334341776006,
0.00322035894802675,0.00360779073578523,0.00370395595929687,0.00429989379062265,
0.00454486050103351,0.00462994494912103,0.00532482870883918,0.00549165268203304,
0.00555593393894519,0.00622533162053515,0.00648192292876935,0.00695499059398613,
0.00740791170339487),.UNSPECIFIED.);
#882=B_SPLINE_CURVE_WITH_KNOTS('',3,(#19684,#19685,#19686,#19687,#19688,
#19689,#19690,#19691,#19692,#19693,#19694,#19695,#19696,#19697,#19698,#19699,
#19700,#19701,#19702,#19703,#19704,#19705,#19706,#19707,#19708,#19709,#19710,
#19711,#19712,#19713,#19714,#19715,#19716,#19717,#19718,#19719,#19720,#19721,
#19722,#19723,#19724,#19725,#19726,#19727,#19728,#19729,#19730,#19731,#19732,
#19733,#19734,#19735,#19736,#19737,#19738,#19739,#19740,#19741,#19742,#19743,
#19744,#19745,#19746,#19747,#19748,#19749,#19750),.UNSPECIFIED.,.F.,.F.,
(4,3,3,3,3,3,3,3,3,3,3,3,3,3,3,3,3,3,3,3,3,3,4),(-1.26412812962169E-5,0.000494289993516549,
0.000916182220770617,0.00158761602821044,0.00184500593803732,0.00190945524103177,
0.00260645980420792,0.00277382965530402,0.00285915079249246,0.00345690366729172,
0.00370265337257072,0.00379909409684229,0.00427723699929272,0.00473898476131605,
0.00517836782884145,0.00556030080710405,0.00563986899627211,0.00601852659233303,
0.00638213905693613,0.00648912452437073,0.00685144713428646,0.00721253712890148,
0.00741794824163741),.UNSPECIFIED.);
#883=B_SPLINE_CURVE_WITH_KNOTS('',3,(#19752,#19753,#19754,#19755,#19756,
#19757),.UNSPECIFIED.,.F.,.F.,(4,2,4),(0.,0.00170403531088726,0.00340807062177452),
 .UNSPECIFIED.);
#884=B_SPLINE_CURVE_WITH_KNOTS('',3,(#19760,#19761,#19762,#19763,#19764,
#19765,#19766,#19767,#19768,#19769,#19770,#19771,#19772,#19773,#19774,#19775),
 .UNSPECIFIED.,.F.,.F.,(4,2,2,2,2,2,2,4),(0.00340807062177452,0.00495591214335585,
0.00650375366493717,0.0080515951865185,0.00959943670809982,0.0111472782296811,
0.0126951197512625,0.0157908027944251),.UNSPECIFIED.);
#885=B_SPLINE_CURVE_WITH_KNOTS('',3,(#19777,#19778,#19779,#19780,#19781,
#19782,#19783,#19784,#19785,#19786,#19787,#19788,#19789,#19790,#19791,#19792,
#19793,#19794,#19795,#19796,#19797,#19798,#19799,#19800,#19801,#19802,#19803,
#19804,#19805,#19806,#19807,#19808,#19809,#19810,#19811,#19812,#19813,#19814,
#19815,#19816,#19817,#19818,#19819,#19820,#19821,#19822,#19823,#19824,#19825,
#19826,#19827,#19828,#19829,#19830,#19831,#19832,#19833,#19834,#19835,#19836,
#19837,#19838,#19839,#19840),.UNSPECIFIED.,.F.,.F.,(4,3,3,3,3,3,3,3,3,3,
3,3,3,3,3,3,3,3,3,3,3,4),(0.,0.000217008353627195,0.00044324659857817,0.000652120823339668,
0.000696799127034378,0.0009320141666111,0.00117457155402921,0.00130424164667934,
0.00137662244777993,0.00162564089691921,0.00188989041240164,0.001956362470019,
0.00203919216218315,0.00242993572455044,0.00260848329335867,0.00268907034510375,
0.00324577551876228,0.00378706053238822,0.00391272494003789,0.0039649107976047,
0.00469438531296503,0.0052169665867171),.UNSPECIFIED.);
#886=B_SPLINE_CURVE_WITH_KNOTS('',3,(#19844,#19845,#19846,#19847,#19848,
#19849,#19850,#19851,#19852,#19853,#19854,#19855,#19856,#19857,#19858,#19859,
#19860,#19861,#19862,#19863,#19864,#19865,#19866,#19867,#19868,#19869,#19870,
#19871,#19872,#19873,#19874,#19875,#19876,#19877,#19878,#19879,#19880,#19881,
#19882,#19883,#19884,#19885,#19886,#19887,#19888,#19889,#19890,#19891,#19892,
#19893,#19894,#19895,#19896,#19897,#19898,#19899,#19900,#19901,#19902,#19903,
#19904,#19905,#19906,#19907,#19908,#19909,#19910,#19911,#19912,#19913),
 .UNSPECIFIED.,.F.,.F.,(4,3,3,3,3,3,3,3,3,3,3,3,3,3,3,3,3,3,3,3,3,3,3,4),
(0.,0.000716363515082861,0.00122272058882501,0.00127670474543072,0.001684939739755,
0.00184333900175369,0.001915057118146,0.0022617033425768,0.00247119369116529,
0.00255340949086129,0.00284871880498323,0.00310811407391612,0.00319176186357658,
0.00345491419006973,0.00370405315221264,0.00375758515241602,0.00383011423629186,
0.00419648947130024,0.00442380729262466,0.00446846660900715,0.00466401696562969,
0.00485470026116451,0.00503802593101401,0.00510681898172244),
 .UNSPECIFIED.);
#887=B_SPLINE_CURVE_WITH_KNOTS('',3,(#19914,#19915,#19916,#19917,#19918,
#19919,#19920,#19921,#19922,#19923,#19924,#19925,#19926,#19927,#19928,#19929,
#19930,#19931),.UNSPECIFIED.,.F.,.F.,(4,2,2,2,2,2,2,2,4),(0.,0.003068525446753,
0.0046027881701295,0.00613705089350601,0.00767131361688251,0.00843844497857076,
0.00920557634025901,0.0107398390636356,0.0122741017870122),
 .UNSPECIFIED.);
#888=B_SPLINE_CURVE_WITH_KNOTS('',3,(#19945,#19946,#19947,#19948,#19949,
#19950,#19951,#19952,#19953,#19954,#19955,#19956,#19957,#19958,#19959,#19960,
#19961,#19962,#19963,#19964,#19965,#19966,#19967,#19968,#19969,#19970,#19971,
#19972,#19973,#19974,#19975,#19976,#19977,#19978,#19979,#19980,#19981,#19982,
#19983,#19984,#19985,#19986,#19987,#19988,#19989,#19990),.UNSPECIFIED.,
 .F.,.F.,(4,3,3,3,3,3,3,3,3,3,3,3,3,3,3,4),(0.,0.00135730202997046,0.00181088490961025,
0.00181523918786338,0.00271632736441538,0.00272329467697279,0.00362176981922051,
0.00363238660702296,0.00452721227402563,0.00454314116852505,0.00525055669087674,
0.00543265472883076,0.00545594202104736,0.0062798042883095,0.00708587073896267,
0.00724353963844092),.UNSPECIFIED.);
#889=B_SPLINE_CURVE_WITH_KNOTS('',3,(#19991,#19992,#19993,#19994,#19995,
#19996,#19997,#19998,#19999,#20000,#20001,#20002,#20003,#20004,#20005,#20006,
#20007,#20008,#20009,#20010,#20011,#20012,#20013,#20014,#20015,#20016,#20017,
#20018,#20019,#20020,#20021,#20022,#20023,#20024,#20025,#20026,#20027,#20028,
#20029,#20030,#20031,#20032,#20033,#20034,#20035,#20036),.UNSPECIFIED.,
 .F.,.F.,(4,3,3,3,3,3,3,3,3,3,3,3,3,3,3,4),(0.,0.000808445975810305,0.00163472102823258,
0.00179462353986192,0.00181800235978474,0.00252819829650182,0.00271101203870707,
0.00272700353967716,0.00362534620384845,0.00363600471956958,0.00453801120277895,
0.00454500589946201,0.00544963568717067,0.00545400707935443,0.00681664400249974,
0.00727200943913927),.UNSPECIFIED.);
#890=B_SPLINE_CURVE_WITH_KNOTS('',3,(#20241,#20242,#20243,#20244),
 .UNSPECIFIED.,.F.,.F.,(4,4),(5.7219584981528E-17,0.00198881562236583),
 .UNSPECIFIED.);
#891=B_SPLINE_CURVE_WITH_KNOTS('',3,(#20248,#20249,#20250,#20251,#20252,
#20253,#20254,#20255,#20256,#20257,#20258,#20259,#20260,#20261,#20262,#20263,
#20264,#20265,#20266,#20267,#20268,#20269,#20270,#20271,#20272,#20273,#20274,
#20275,#20276,#20277,#20278,#20279,#20280,#20281,#20282,#20283,#20284,#20285,
#20286,#20287,#20288,#20289,#20290,#20291,#20292,#20293,#20294,#20295,#20296,
#20297,#20298,#20299,#20300,#20301,#20302,#20303,#20304,#20305,#20306,#20307,
#20308,#20309,#20310,#20311,#20312,#20313,#20314,#20315,#20316,#20317,#20318,
#20319,#20320,#20321,#20322,#20323,#20324,#20325,#20326,#20327,#20328,#20329),
 .UNSPECIFIED.,.F.,.F.,(4,3,3,3,3,3,3,3,3,3,3,3,3,3,3,3,3,3,3,3,3,3,3,3,
3,3,3,4),(1.2719202621569E-16,0.00143589979508649,0.00284404218546533,0.00415362629242205,
0.0042305644511401,0.00504888151365028,0.00519203286552742,0.00527815489686518,
0.00614833446736157,0.00623043943863279,0.00632123327719083,0.00726884601173815,
0.00735976193107753,0.0080560493804554,0.00830725258484352,0.00839384909481171,
0.00982686164286283,0.0103840657310542,0.0104535759650963,0.0114224723041596,
0.0114795275119261,0.0120957876665379,0.012460878877265,0.012503118356934,
0.0135294573324798,0.0145557963080255,0.015608619261337,0.0166145051696864),
 .UNSPECIFIED.);
#892=B_SPLINE_CURVE_WITH_KNOTS('',3,(#20334,#20335,#20336,#20337),
 .UNSPECIFIED.,.F.,.F.,(4,4),(0.,0.00198881562236589),.UNSPECIFIED.);
#893=B_SPLINE_CURVE_WITH_KNOTS('',3,(#20339,#20340,#20341,#20342,#20343,
#20344,#20345,#20346,#20347,#20348,#20349,#20350,#20351,#20352,#20353,#20354,
#20355,#20356,#20357,#20358,#20359,#20360,#20361,#20362,#20363,#20364,#20365,
#20366,#20367,#20368,#20369,#20370,#20371,#20372,#20373,#20374,#20375,#20376,
#20377,#20378,#20379,#20380,#20381,#20382,#20383,#20384,#20385,#20386,#20387,
#20388,#20389,#20390,#20391,#20392,#20393,#20394,#20395,#20396,#20397,#20398,
#20399,#20400,#20401,#20402,#20403,#20404,#20405,#20406,#20407,#20408,#20409,
#20410,#20411,#20412,#20413,#20414,#20415,#20416,#20417,#20418,#20419,#20420,
#20421,#20422,#20423),.UNSPECIFIED.,.F.,.F.,(4,3,3,3,3,3,3,3,3,3,3,3,3,
3,3,3,3,3,3,3,3,3,3,3,3,3,3,3,4),(0.,0.000716458183822177,0.00142634914675041,
0.00205206754060844,0.0020932945390166,0.00296723761715126,0.00308523603842144,
0.00313994180852491,0.00377181010115693,0.00411797980288768,0.00418658907803322,
0.00581684750097351,0.00618890273310859,0.00627988361704989,0.0070571831999972,
0.0072274457512027,0.00732653088655817,0.00795375102207312,0.00826812044930995,
0.00837317815606645,0.00945419362478756,0.0105567220809739,0.0116943447997248,
0.0124737944199864,0.0125597672340995,0.0136064145036077,0.0146658962125278,
0.0157534067466141,0.0167463563121324),.UNSPECIFIED.);
#894=B_SPLINE_CURVE_WITH_KNOTS('',3,(#20471,#20472,#20473,#20474,#20475,
#20476,#20477,#20478,#20479,#20480,#20481,#20482,#20483,#20484,#20485,#20486,
#20487,#20488,#20489,#20490,#20491,#20492,#20493,#20494,#20495,#20496,#20497,
#20498,#20499,#20500,#20501,#20502,#20503,#20504,#20505,#20506,#20507,#20508,
#20509,#20510,#20511,#20512,#20513,#20514,#20515,#20516,#20517,#20518,#20519,
#20520,#20521,#20522,#20523,#20524,#20525,#20526,#20527,#20528,#20529,#20530,
#20531,#20532,#20533,#20534,#20535,#20536,#20537,#20538,#20539,#20540,#20541,
#20542,#20543,#20544,#20545,#20546),.UNSPECIFIED.,.F.,.F.,(4,3,3,3,3,3,
3,3,3,3,3,3,3,3,3,3,3,3,3,3,3,3,3,3,3,4),(2.77988148204925E-13,0.000240598629271839,
0.000486088690534841,0.000739379865323794,0.00086351953650479,0.00109201081567983,
0.00132914312091213,0.00138485296015832,0.00163896000397727,0.00172703907300957,
0.0020510032560785,0.0023836347224887,0.0027322580415582,0.00302289580528531,
0.00335373644476616,0.00345407814601918,0.00382021337536123,0.00392909696477702,
0.00441388534005964,0.00488365632772136,0.00518111721902879,0.00572151392286165,
0.00604463675553361,0.00642122800801736,0.00679034626207549,0.006908156208912),
 .UNSPECIFIED.);
#895=B_SPLINE_CURVE_WITH_KNOTS('',3,(#20640,#20641,#20642,#20643,#20644,
#20645,#20646,#20647,#20648,#20649,#20650,#20651,#20652,#20653,#20654,#20655,
#20656,#20657,#20658,#20659,#20660,#20661,#20662,#20663,#20664,#20665,#20666,
#20667,#20668,#20669,#20670,#20671,#20672,#20673,#20674,#20675,#20676,#20677,
#20678,#20679,#20680,#20681,#20682,#20683,#20684,#20685,#20686,#20687,#20688,
#20689,#20690,#20691,#20692,#20693,#20694,#20695,#20696,#20697,#20698,#20699,
#20700,#20701,#20702,#20703,#20704,#20705,#20706,#20707,#20708,#20709,#20710,
#20711,#20712,#20713,#20714,#20715,#20716,#20717,#20718),.UNSPECIFIED.,
 .F.,.F.,(4,3,3,3,3,3,3,3,3,3,3,3,3,3,3,3,3,3,3,3,3,3,3,3,3,3,4),(0.,7.02681003220256E-5,
0.000143250041041023,0.000221865135200779,0.000253452295756187,0.000331299522547507,
0.000365730675067348,0.000448634730986367,0.000506904591512373,0.00060316276770857,
0.000705610759866986,0.000806172107809853,0.000924817647814786,0.00101380918302463,
0.00117169973492681,0.00130438666521286,0.00150431742405288,0.00171807903281978,
0.00183569921664511,0.00202761836604909,0.00233306873065422,0.00238482361429225,
0.00276944460394528,0.00293994271643501,0.00304142754907356,0.00391372248518797,
0.00405523673209802),.UNSPECIFIED.);
#896=B_SPLINE_CURVE_WITH_KNOTS('',3,(#20773,#20774,#20775,#20776,#20777,
#20778,#20779,#20780,#20781,#20782,#20783,#20784,#20785,#20786,#20787,#20788,
#20789,#20790,#20791,#20792,#20793,#20794,#20795,#20796,#20797,#20798,#20799,
#20800,#20801,#20802,#20803,#20804,#20805,#20806,#20807,#20808,#20809,#20810,
#20811,#20812,#20813,#20814,#20815,#20816,#20817,#20818,#20819,#20820,#20821,
#20822,#20823,#20824,#20825,#20826,#20827,#20828,#20829,#20830,#20831,#20832,
#20833,#20834,#20835,#20836,#20837,#20838,#20839,#20840,#20841,#20842,#20843,
#20844,#20845,#20846,#20847,#20848,#20849,#20850,#20851),.UNSPECIFIED.,
 .F.,.F.,(4,3,3,3,3,3,3,3,3,3,3,3,3,3,3,3,3,3,3,3,3,3,3,3,3,3,4),(0.,0.000574140202871799,
0.00100221889234342,0.00110612621604268,0.0015045731206471,0.00187271135781319,
0.00200443778468684,0.0021955000540258,0.00239948716108467,0.00258607856328849,
0.00272128426511772,0.0028703854494012,0.00300665667703026,0.00311994789192807,
0.0032136798020773,0.00331311536984171,0.00341044074652188,0.00350046922160291,
0.00350776612320204,0.00359009987782602,0.00364838382063052,0.00372718996528856,
0.0037583208462879,0.00382357344841964,0.00388604433371314,0.00394745995154345,
0.00400887556937376),.UNSPECIFIED.);
#897=B_SPLINE_CURVE_WITH_KNOTS('',3,(#20894,#20895,#20896,#20897,#20898,
#20899,#20900,#20901,#20902,#20903,#20904,#20905,#20906,#20907,#20908,#20909,
#20910,#20911,#20912,#20913,#20914,#20915,#20916,#20917,#20918,#20919,#20920,
#20921,#20922,#20923,#20924,#20925,#20926,#20927,#20928,#20929,#20930,#20931,
#20932,#20933,#20934,#20935,#20936,#20937,#20938,#20939,#20940,#20941,#20942,
#20943,#20944,#20945,#20946,#20947,#20948,#20949,#20950,#20951,#20952,#20953,
#20954,#20955,#20956,#20957,#20958,#20959,#20960,#20961,#20962,#20963,#20964,
#20965,#20966,#20967,#20968,#20969),.UNSPECIFIED.,.F.,.F.,(4,3,3,3,3,3,
3,3,3,3,3,3,3,3,3,3,3,3,3,3,3,3,3,3,3,4),(-1.6328271194595E-5,0.000369433773630129,
0.000757274070195943,0.000848560634670326,0.00138981505096866,0.00171344962366214,
0.00201136389971158,0.00249692265816024,0.00296744070560773,0.00333415714234072,
0.00344322760164585,0.00377459389855988,0.00387508241180588,0.00422407835213338,
0.00456272284537112,0.00488624813330148,0.00517300557962956,0.00542751638642631,
0.00551572915222377,0.00575380985097023,0.00598306732204141,0.00603789456862142,
0.00629079704341219,0.00653838705347384,0.00677847963654176,0.00690278355733486),
 .UNSPECIFIED.);
#898=B_SPLINE_CURVE_WITH_KNOTS('',3,(#21135,#21136,#21137,#21138,#21139,
#21140,#21141,#21142,#21143,#21144),.UNSPECIFIED.,.F.,.F.,(4,2,2,2,4),(-1.46797143552028,
-1.30470040394833,-1.06055016507708,-0.816399926205828,-0.65312889463391),
 .UNSPECIFIED.);
#899=B_SPLINE_CURVE_WITH_KNOTS('',3,(#21152,#21153,#21154,#21155,#21156,
#21157,#21158,#21159,#21160,#21161),.UNSPECIFIED.,.F.,.F.,(4,2,2,2,4),(0.653128894633879,
0.816399926205827,1.06055016507708,1.30470040394833,1.46797143552025),
 .UNSPECIFIED.);
#900=B_SPLINE_CURVE_WITH_KNOTS('',3,(#21164,#21165,#21166,#21167,#21168,
#21169,#21170,#21171,#21172,#21173,#21174,#21175,#21176,#21177,#21178,#21179),
 .UNSPECIFIED.,.F.,.F.,(4,2,2,2,2,2,2,4),(1.82537904839244,2.10770426762789,
2.46113598680775,2.81456770598761,3.16799942516747,3.52143114434733,3.87164135166438,
4.22185155898142),.UNSPECIFIED.);
#901=B_SPLINE_CURVE_WITH_KNOTS('',3,(#21183,#21184,#21185,#21186,#21187,
#21188,#21189,#21190,#21191,#21192,#21193,#21194,#21195,#21196,#21197,#21198,
#21199),.UNSPECIFIED.,.F.,.F.,(4,2,2,2,3,2,2,4),(4.22185155898142,4.57206176629846,
4.92227197361551,5.27570369279537,5.62913541197523,5.98256713115509,6.33599885033495,
6.61832406957041),.UNSPECIFIED.);
#902=B_SPLINE_CURVE_WITH_KNOTS('',3,(#21205,#21206,#21207,#21208,#21209,
#21210,#21211,#21212,#21213,#21214,#21215,#21216,#21217,#21218,#21219,#21220),
 .UNSPECIFIED.,.F.,.F.,(4,2,2,2,2,2,2,4),(1.40728385299381,1.75749406031085,
2.10770426762789,2.46113598680775,2.81456770598761,3.16799942516747,3.52143114434734,
3.8037563635828),.UNSPECIFIED.);
#903=B_SPLINE_CURVE_WITH_KNOTS('',3,(#21221,#21222,#21223,#21224,#21225,
#21226,#21227,#21228,#21229,#21230,#21231,#21232,#21233,#21234,#21235,#21236,
#21237),.UNSPECIFIED.,.F.,.F.,(4,2,2,3,2,2,2,4),(-0.989188657595171,-0.706863438359723,
-0.353431719179861,8.88178419700125E-16,0.353431719179861,0.706863438359721,
1.05707364567676,1.40728385299381),.UNSPECIFIED.);
#904=B_SPLINE_CURVE_WITH_KNOTS('',3,(#21510,#21511,#21512,#21513,#21514,
#21515,#21516,#21517,#21518,#21519,#21520,#21521,#21522,#21523,#21524,#21525,
#21526,#21527,#21528,#21529,#21530,#21531,#21532,#21533,#21534,#21535,#21536,
#21537,#21538,#21539,#21540,#21541,#21542,#21543,#21544,#21545,#21546,#21547),
 .UNSPECIFIED.,.F.,.F.,(4,2,2,2,2,2,2,2,2,2,2,2,2,2,2,2,2,2,4),(1.00089634517109E-6,
0.0135124805886909,0.0270102893796787,0.0542554527433717,0.0725924484028551,
0.0831509031929542,0.0939203394783847,0.114150905777324,0.132564433691206,
0.163148633358063,0.193616759129243,0.211927287774423,0.23206669119174,
0.242799260198686,0.253302631405238,0.27156325585088,0.298722401714205,
0.312167688321445,0.325612440221502),.UNSPECIFIED.);
#905=B_SPLINE_CURVE_WITH_KNOTS('',3,(#21551,#21552,#21553,#21554,#21555,
#21556,#21557,#21558,#21559,#21560,#21561,#21562,#21563,#21564,#21565,#21566,
#21567,#21568,#21569,#21570,#21571,#21572),.UNSPECIFIED.,.F.,.F.,(4,2,2,
2,2,2,2,2,2,2,4),(0.,0.0625283246425461,0.0937924869638204,0.125056649285095,
0.187584973927639,0.250113298570183,0.312641623212727,0.343905785533998,
0.359537866694632,0.375169947855267,0.500226597140354),.UNSPECIFIED.);
#906=B_SPLINE_CURVE_WITH_KNOTS('',3,(#21612,#21613,#21614,#21615,#21616,
#21617,#21618,#21619,#21620,#21621,#21622,#21623,#21624,#21625,#21626,#21627,
#21628,#21629,#21630,#21631,#21632,#21633,#21634,#21635,#21636,#21637,#21638,
#21639,#21640,#21641,#21642,#21643,#21644,#21645,#21646,#21647,#21648,#21649),
 .UNSPECIFIED.,.F.,.F.,(4,2,2,2,2,2,2,2,2,2,2,2,2,2,2,2,2,2,4),(1.00089547843557E-6,
0.0135124805885893,0.0270102893791961,0.0542554527419749,0.072592448400889,
0.0831509031907464,0.0939203394761004,0.1141509057748,0.132564433688463,
0.163148633354892,0.193616759125631,0.211927287770558,0.232066691187639,
0.242799260194547,0.253302631400942,0.271563255846155,0.298722401708962,
0.312167688315685,0.325612440214992),.UNSPECIFIED.);
#907=B_SPLINE_CURVE_WITH_KNOTS('',3,(#21653,#21654,#21655,#21656,#21657,
#21658,#21659,#21660,#21661,#21662,#21663,#21664,#21665,#21666,#21667,#21668,
#21669,#21670,#21671,#21672,#21673,#21674),.UNSPECIFIED.,.F.,.F.,(4,2,2,
2,2,2,2,2,2,2,4),(0.,0.0625305420531017,0.0937958130796483,0.125061084106195,
0.187591626159283,0.250122168212371,0.31265271026546,0.343917981292008,
0.359550616805279,0.37518325231855,0.500244336424745),.UNSPECIFIED.);
#908=B_SPLINE_CURVE_WITH_KNOTS('',3,(#21677,#21678,#21679,#21680,#21681,
#21682,#21683,#21684,#21685,#21686,#21687,#21688,#21689,#21690,#21691,#21692,
#21693,#21694,#21695,#21696,#21697,#21698,#21699,#21700,#21701,#21702,#21703,
#21704,#21705,#21706,#21707,#21708,#21709,#21710,#21711,#21712,#21713,#21714),
 .UNSPECIFIED.,.F.,.F.,(4,2,2,2,2,2,2,2,2,2,2,2,2,2,2,2,2,2,4),(0.,0.0303468331885949,
0.0404805816100016,0.0838349998679533,0.0899468517242951,0.0960856059764287,
0.119205002215768,0.140283020185445,0.159234503235151,0.176557837747224,
0.209013384982688,0.227277173706207,0.247357834439419,0.25806173913776,
0.268531153677092,0.286711917123732,0.300273063907743,0.310385248581606,
0.340667271090375),.UNSPECIFIED.);
#909=B_SPLINE_CURVE_WITH_KNOTS('',3,(#21716,#21717,#21718,#21719,#21720,
#21721,#21722,#21723,#21724,#21725,#21726,#21727,#21728,#21729,#21730,#21731,
#21732,#21733,#21734,#21735,#21736,#21737,#21738,#21739,#21740,#21741,#21742,
#21743,#21744,#21745,#21746,#21747,#21748,#21749,#21750,#21751,#21752,#21753),
 .UNSPECIFIED.,.F.,.F.,(4,2,2,2,2,2,2,2,2,2,2,2,2,2,2,2,2,2,4),(0.,0.0303468331885437,
0.0404805816098057,0.0838349998664512,0.0899468517228076,0.096085605973945,
0.119205002207746,0.140283020172398,0.159234503217531,0.176557837725533,
0.209013384952252,0.227277173670161,0.247357834397049,0.258061739092016,
0.268531153628422,0.286711917069987,0.300273063850531,0.310385248521581,
0.340667271021422),.UNSPECIFIED.);
#910=B_SPLINE_CURVE_WITH_KNOTS('',3,(#21764,#21765,#21766,#21767,#21768,
#21769,#21770,#21771,#21772,#21773,#21774,#21775,#21776,#21777,#21778,#21779,
#21780,#21781,#21782,#21783,#21784,#21785),.UNSPECIFIED.,.F.,.F.,(4,2,2,
2,2,2,2,2,2,2,4),(0.500226597140354,0.562698272497809,0.593934110176538,
0.625169947855266,0.687641623212725,0.750113298570185,0.812584973927644,
0.843820811606377,0.859438730445742,0.875056649285107,1.),.UNSPECIFIED.);
#911=B_SPLINE_CURVE_WITH_KNOTS('',3,(#21786,#21787,#21788,#21789,#21790,
#21791,#21792,#21793,#21794,#21795,#21796,#21797,#21798,#21799,#21800,#21801,
#21802,#21803,#21804,#21805,#21806,#21807,#21808,#21809),.UNSPECIFIED.,
 .F.,.F.,(4,2,2,2,2,2,2,2,2,2,2,4),(0.500244336424745,0.56271379437167,
0.593948523345132,0.609565887831865,0.625183252318598,0.687652710265505,
0.750122168212412,0.812591626159318,0.843826355132767,0.859443719619489,
0.87506108410621,1.),.UNSPECIFIED.);
#912=B_SPLINE_CURVE_WITH_KNOTS('',3,(#21939,#21940,#21941,#21942,#21943,
#21944,#21945,#21946,#21947,#21948,#21949,#21950,#21951,#21952,#21953,#21954,
#21955,#21956,#21957,#21958,#21959,#21960,#21961,#21962,#21963,#21964,#21965,
#21966,#21967,#21968,#21969,#21970,#21971,#21972,#21973,#21974,#21975,#21976),
 .UNSPECIFIED.,.F.,.F.,(4,2,2,2,2,2,2,2,2,2,2,2,2,2,2,2,2,2,4),(1.00089633934029E-6,
0.0135124805888077,0.0270102893800241,0.0542554527437976,0.0725924484033422,
0.0831509031934888,0.0939203394789252,0.114150905777859,0.132564433691779,
0.163148633358663,0.193616759129903,0.211927287775115,0.232066691192426,
0.242799260199493,0.253302631405774,0.271563255850625,0.298722401712991,
0.312167688319558,0.32561244021873),.UNSPECIFIED.);
#913=B_SPLINE_CURVE_WITH_KNOTS('',3,(#21980,#21981,#21982,#21983,#21984,
#21985,#21986,#21987,#21988,#21989,#21990,#21991,#21992,#21993,#21994,#21995,
#21996,#21997,#21998,#21999,#22000,#22001),.UNSPECIFIED.,.F.,.F.,(4,2,2,
2,2,2,2,2,2,2,4),(0.,0.062528324642553,0.0937924869638229,0.125056649285093,
0.187584973927634,0.250113298570175,0.312641623212717,0.343905785533987,
0.359537866694625,0.375169947855263,0.500226597140362),.UNSPECIFIED.);
#914=B_SPLINE_CURVE_WITH_KNOTS('',3,(#22041,#22042,#22043,#22044,#22045,
#22046,#22047,#22048,#22049,#22050,#22051,#22052,#22053,#22054,#22055,#22056,
#22057,#22058,#22059,#22060,#22061,#22062,#22063,#22064,#22065,#22066,#22067,
#22068,#22069,#22070,#22071,#22072,#22073,#22074,#22075,#22076,#22077,#22078),
 .UNSPECIFIED.,.F.,.F.,(4,2,2,2,2,2,2,2,2,2,2,2,2,2,2,2,2,2,4),(1.00089547198642E-6,
0.0135124805886458,0.0270102893792894,0.0542554527414999,0.0725924484001046,
0.0831509031898948,0.0939203394752058,0.114150905773714,0.132564433687167,
0.163148633353336,0.193616759123885,0.211927287768641,0.232066691185389,
0.242799260192144,0.253302631398652,0.27156325584398,0.29872240170682,0.312167688313921,
0.32561244021362),.UNSPECIFIED.);
#915=B_SPLINE_CURVE_WITH_KNOTS('',3,(#22082,#22083,#22084,#22085,#22086,
#22087,#22088,#22089,#22090,#22091,#22092,#22093,#22094,#22095,#22096,#22097,
#22098,#22099,#22100,#22101,#22102,#22103),.UNSPECIFIED.,.F.,.F.,(4,2,2,
2,2,2,2,2,2,2,4),(0.,0.0625305420531068,0.0937958130796515,0.125061084106196,
0.187591626159282,0.250122168212368,0.312652710265454,0.343917981291998,
0.359550616805267,0.375183252318535,0.500244336424746),.UNSPECIFIED.);
#916=B_SPLINE_CURVE_WITH_KNOTS('',3,(#22106,#22107,#22108,#22109,#22110,
#22111,#22112,#22113,#22114,#22115,#22116,#22117,#22118,#22119,#22120,#22121,
#22122,#22123,#22124,#22125,#22126,#22127,#22128,#22129,#22130,#22131,#22132,
#22133,#22134,#22135,#22136,#22137,#22138,#22139,#22140,#22141,#22142,#22143),
 .UNSPECIFIED.,.F.,.F.,(4,2,2,2,2,2,2,2,2,2,2,2,2,2,2,2,2,2,4),(0.,0.0303468331886201,
0.0404805816100005,0.0838349998685196,0.0899468517249421,0.0960856059763945,
0.119205002212153,0.140283020178524,0.159234503225117,0.176557837734437,
0.209013384964693,0.227277173685149,0.247357834414858,0.25806173911128,
0.268531153648718,0.286711917091893,0.300273063873447,0.310385248545583,
0.340667271049151),.UNSPECIFIED.);
#917=B_SPLINE_CURVE_WITH_KNOTS('',3,(#22145,#22146,#22147,#22148,#22149,
#22150,#22151,#22152,#22153,#22154,#22155,#22156,#22157,#22158,#22159,#22160,
#22161,#22162,#22163,#22164,#22165,#22166,#22167,#22168,#22169,#22170,#22171,
#22172,#22173,#22174,#22175,#22176,#22177,#22178,#22179,#22180,#22181,#22182),
 .UNSPECIFIED.,.F.,.F.,(4,2,2,2,2,2,2,2,2,2,2,2,2,2,2,2,2,2,4),(0.,0.0303468331885424,
0.0404805816097377,0.0838349998665984,0.0899468517222195,0.0960856059733606,
0.119205002209305,0.140283020175775,0.159234503222523,0.176557837732021,
0.209013384962109,0.227277173682202,0.247357834411472,0.258061739107788,
0.268531153645427,0.28671191708922,0.300273063871285,0.310385248543308,
0.340667271045991),.UNSPECIFIED.);
#918=B_SPLINE_CURVE_WITH_KNOTS('',3,(#22193,#22194,#22195,#22196,#22197,
#22198,#22199,#22200,#22201,#22202,#22203,#22204,#22205,#22206,#22207,#22208,
#22209,#22210,#22211,#22212,#22213,#22214),.UNSPECIFIED.,.F.,.F.,(4,2,2,
2,2,2,2,2,2,2,4),(0.500226597140362,0.562698272497811,0.593934110176537,
0.625169947855262,0.687641623212722,0.750113298570183,0.812584973927644,
0.843820811606372,0.859438730445736,0.875056649285099,1.),.UNSPECIFIED.);
#919=B_SPLINE_CURVE_WITH_KNOTS('',3,(#22215,#22216,#22217,#22218,#22219,
#22220,#22221,#22222,#22223,#22224,#22225,#22226,#22227,#22228,#22229,#22230,
#22231,#22232,#22233,#22234,#22235,#22236,#22237,#22238),.UNSPECIFIED.,
 .F.,.F.,(4,2,2,2,2,2,2,2,2,2,2,4),(0.500244336424746,0.562713794371627,
0.593948523345067,0.609565887831793,0.625183252318519,0.687652710265425,
0.75012216821233,0.812591626159236,0.843826355132694,0.859443719619418,
0.875061084106143,1.),.UNSPECIFIED.);
#920=B_SPLINE_CURVE_WITH_KNOTS('',3,(#22599,#22600,#22601,#22602,#22603,
#22604,#22605,#22606,#22607,#22608,#22609,#22610,#22611),.UNSPECIFIED.,
 .F.,.F.,(4,3,3,3,4),(-8.94491631300586E-6,0.000122293976412443,0.000196963243301103,
0.000348477111734026,0.000402871401407367),.UNSPECIFIED.);
#921=B_SPLINE_CURVE_WITH_KNOTS('',3,(#22635,#22636,#22637,#22638,#22639,
#22640,#22641,#22642,#22643,#22644,#22645,#22646,#22647),.UNSPECIFIED.,
 .F.,.F.,(4,3,3,3,4),(1.90501246655379E-12,0.000149886598358764,0.000203002185902805,
0.000344863019354018,0.000406004371347535),.UNSPECIFIED.);
#922=B_SPLINE_CURVE_WITH_KNOTS('',3,(#22716,#22717,#22718,#22719,#22720,
#22721,#22722,#22723,#22724,#22725,#22726,#22727,#22728,#22729,#22730,#22731,
#22732,#22733,#22734,#22735,#22736,#22737,#22738,#22739,#22740,#22741,#22742,
#22743,#22744,#22745,#22746,#22747,#22748,#22749,#22750,#22751,#22752,#22753,
#22754,#22755,#22756,#22757,#22758,#22759,#22760,#22761),.UNSPECIFIED.,
 .F.,.F.,(4,2,2,2,2,2,2,2,2,2,2,2,2,2,2,2,2,2,2,2,2,2,4),(0.,0.00042797836355374,
0.00085595672710748,0.00171191345421505,0.00256787018132261,0.00342382690843018,
0.00513574036264529,0.00684765381686041,0.00770361054396788,0.00855956727107535,
0.0102714807252903,0.0119833941795052,0.0136953076337201,0.0171191345421499,
0.0188310479963648,0.0205429614505798,0.0222548749047947,0.0239667883590096,
0.0248227450861171,0.0256787018132246,0.0265346585403321,0.0269626369038859,
0.0273906152674397),.UNSPECIFIED.);
#923=B_SPLINE_CURVE_WITH_KNOTS('',3,(#22766,#22767,#22768,#22769,#22770,
#22771,#22772,#22773,#22774,#22775,#22776,#22777,#22778,#22779,#22780,#22781,
#22782,#22783,#22784,#22785,#22786,#22787,#22788,#22789,#22790,#22791,#22792,
#22793,#22794,#22795,#22796,#22797,#22798,#22799,#22800,#22801,#22802,#22803,
#22804,#22805,#22806,#22807,#22808,#22809,#22810,#22811,#22812,#22813,#22814,
#22815,#22816,#22817,#22818,#22819,#22820,#22821,#22822,#22823,#22824,#22825,
#22826,#22827,#22828,#22829,#22830,#22831,#22832,#22833,#22834,#22835,#22836,
#22837,#22838,#22839,#22840,#22841,#22842,#22843,#22844,#22845,#22846,#22847,
#22848,#22849,#22850,#22851,#22852,#22853,#22854,#22855,#22856,#22857,#22858,
#22859,#22860,#22861,#22862,#22863,#22864,#22865,#22866,#22867,#22868,#22869,
#22870,#22871,#22872,#22873,#22874,#22875,#22876,#22877,#22878,#22879,#22880,
#22881,#22882,#22883,#22884,#22885,#22886,#22887,#22888,#22889,#22890,#22891,
#22892,#22893,#22894,#22895,#22896,#22897,#22898,#22899,#22900,#22901,#22902,
#22903,#22904,#22905,#22906,#22907,#22908,#22909,#22910,#22911,#22912,#22913,
#22914,#22915,#22916,#22917,#22918,#22919,#22920,#22921,#22922,#22923,#22924,
#22925,#22926,#22927,#22928,#22929,#22930,#22931,#22932,#22933,#22934,#22935,
#22936,#22937,#22938,#22939,#22940,#22941,#22942,#22943,#22944,#22945,#22946,
#22947,#22948,#22949,#22950,#22951,#22952,#22953,#22954,#22955,#22956,#22957,
#22958,#22959,#22960,#22961,#22962,#22963,#22964,#22965,#22966,#22967,#22968,
#22969,#22970,#22971,#22972,#22973,#22974,#22975,#22976,#22977,#22978,#22979,
#22980,#22981,#22982,#22983,#22984,#22985,#22986,#22987,#22988,#22989,#22990,
#22991,#22992,#22993,#22994,#22995,#22996,#22997,#22998,#22999,#23000),
 .UNSPECIFIED.,.F.,.F.,(4,3,3,3,3,3,3,3,3,3,3,3,3,3,3,3,3,3,3,3,3,3,3,3,
3,3,3,3,3,3,3,3,3,3,3,3,3,3,3,3,3,3,3,3,3,3,3,3,3,3,3,3,3,3,3,3,3,3,3,3,
3,3,3,3,3,3,3,3,3,3,3,3,3,3,3,3,3,3,4),(4.92899567643811E-13,6.25324094450888E-5,
0.000108135161089233,0.000169914174680728,0.000216270322178465,0.00030943720716885,
0.000413935938866143,0.000432540644356983,0.000574368182756462,0.000730585733412546,
0.000865081288713848,0.0011111676997501,0.00137115397560176,0.00165280502519303,
0.00173016257742746,0.0021631859889676,0.00262174667632143,0.00312444156864647,
0.00346032515485454,0.00399962729951328,0.00432540644356815,0.00475794708792495,
0.00519048773228175,0.00580087629302463,0.0064255985829778,0.00692065030970915,
0.00756964026772925,0.00822018102493731,0.00865081288713655,0.00908335353149343,
0.00949422462642801,0.00951589417585031,0.0101632105932538,0.0103809754645641,
0.0110451277363797,0.0117441709571396,0.0124097069791447,0.0130727965065704,
0.0137303575905069,0.0138413006194192,0.0145176167184007,0.0151956374788783,
0.0155714631968468,0.0160965814245652,0.0166216819946583,0.0171475979342611,
0.0173016257742743,0.0179650597324343,0.018627559129564,0.0190317883517019,
0.0198298746356556,0.0206344291379891,0.0207619509291294,0.0213868246193969,
0.022007159801814,0.022492113506557,0.0230625131047404,0.0236423945943625,
0.0241817119047142,0.0242222760839846,0.0246853332276435,0.0250873573726984,
0.0254771261541672,0.025844738861123,0.0259524386614121,0.0262218968916945,
0.0264777260220052,0.0267146153189825,0.0268175199501259,0.0269752262516356,
0.0271182846351551,0.0272500605944827,0.0273581957555719,0.0274515657429817,
0.0274663309166611,0.0275422189045734,0.0275744660777502,0.027633797106646,
0.0276826012383845),.UNSPECIFIED.);
#924=B_SPLINE_CURVE_WITH_KNOTS('',3,(#23891,#23892,#23893,#23894,#23895,
#23896,#23897,#23898,#23899,#23900,#23901,#23902,#23903,#23904,#23905,#23906,
#23907,#23908,#23909,#23910,#23911,#23912,#23913,#23914,#23915,#23916,#23917,
#23918,#23919,#23920,#23921,#23922,#23923,#23924,#23925,#23926),
 .UNSPECIFIED.,.F.,.F.,(4,2,2,2,2,2,2,2,2,2,2,2,2,2,2,2,2,4),(-5.52282176378171,
-5.32896740108138,-5.13535365951528,-4.93516142497304,-4.74154376120979,
-4.5415111268812,-4.34788553839797,-4.14801905426253,-3.95438131120499,
-3.75468774664587,-3.56103338796945,-3.36151970744337,-3.16784403857256,
-2.96851737109845,-2.77481546338195,-2.57568306526669,-2.38194975752097,
-2.3652150082907),.UNSPECIFIED.);
#925=B_SPLINE_CURVE_WITH_KNOTS('',3,(#23931,#23932,#23933,#23934,#23935,
#23936,#23937,#23938,#23939,#23940,#23941,#23942,#23943,#23944,#23945,#23946,
#23947,#23948,#23949,#23950,#23951,#23952,#23953,#23954,#23955,#23956,#23957,
#23958),.UNSPECIFIED.,.F.,.F.,(4,2,2,2,2,2,2,2,2,2,2,2,2,4),(-2.3652150082907,
-2.18301896778156,-1.98924887022321,-1.79052705823713,-1.59671455911293,
-1.39820906413684,-1.20434833935788,-1.00606640169784,-0.812151427768874,
-0.614100111573574,-0.420124682089828,-0.222310789965957,-0.110086721669281,
0.),.UNSPECIFIED.);
#926=B_SPLINE_CURVE_WITH_KNOTS('',3,(#23961,#23962,#23963,#23964,#23965,
#23966,#23967,#23968,#23969,#23970,#23971,#23972,#23973,#23974,#23975,#23976,
#23977,#23978,#23979,#23980,#23981,#23982,#23983,#23984,#23985,#23986,#23987,
#23988),.UNSPECIFIED.,.F.,.F.,(4,2,2,2,2,2,2,2,2,2,2,2,2,4),(-37.8682594959783,
-37.6786133520927,-37.4884259218183,-37.2957524665574,-37.0955311656665,
-36.9029287229397,-36.7028085078848,-36.5102760181044,-36.3102600197474,
-36.1177960120006,-35.9178874964689,-35.7254900298269,-35.5256923919229,
-35.5016722138548),.UNSPECIFIED.);
#927=B_SPLINE_CURVE_WITH_KNOTS('',3,(#23993,#23994,#23995,#23996,#23997,
#23998,#23999,#24000,#24001,#24002,#24003,#24004,#24005,#24006,#24007,#24008,
#24009,#24010,#24011,#24012,#24013,#24014,#24015,#24016,#24017,#24018,#24019,
#24020,#24021,#24022,#24023,#24024,#24025,#24026,#24027,#24028),
 .UNSPECIFIED.,.F.,.F.,(4,2,2,2,2,2,2,2,2,2,2,2,2,2,2,2,2,4),(-8.68543777224221,
-8.48472687974919,-8.29102562860789,-8.08976190515885,-7.89608135036397,
-7.69493407611858,-7.50127178683154,-7.30024542791767,-7.10659880541962,
-6.90569808926309,-6.71206435832943,-6.51129427837733,-6.31767047872643,
-6.11703629724468,-5.92341927516968,-5.72292652370587,-5.52931292401888,
-5.52282176378171),.UNSPECIFIED.);
#928=B_SPLINE_CURVE_WITH_KNOTS('',3,(#24029,#24030,#24031,#24032,#24033,
#24034,#24035,#24036,#24037,#24038,#24039,#24040,#24041,#24042,#24043,#24044,
#24045,#24046,#24047,#24048,#24049,#24050,#24051,#24052,#24053,#24054,#24055,
#24056,#24057,#24058,#24059,#24060,#24061,#24062,#24063,#24064),
 .UNSPECIFIED.,.F.,.F.,(4,2,2,2,2,2,2,2,2,2,2,2,2,2,2,2,2,4),(-35.5016722138548,
-35.3333589938397,-35.1336757480503,-34.9414033507716,-34.74183811963,-34.5496229958028,
-34.3501794953646,-34.1580171943271,-33.958699216547,-33.7665845030627,
-33.5673958948966,-33.3753226923794,-33.1762673314815,-32.9842286719963,
-32.7853104389487,-32.5932984224679,-32.3945211695547,-32.3486283723407),
 .UNSPECIFIED.);
#929=B_SPLINE_CURVE_WITH_KNOTS('',3,(#24069,#24070,#24071,#24072,#24073,
#24074,#24075,#24076,#24077,#24078,#24079,#24080,#24081,#24082,#24083,#24084,
#24085,#24086,#24087,#24088,#24089,#24090,#24091,#24092,#24093,#24094,#24095,
#24096,#24097,#24098,#24099,#24100,#24101,#24102,#24103,#24104,#24105,#24106),
 .UNSPECIFIED.,.F.,.F.,(4,2,2,2,2,2,2,2,2,2,2,2,2,2,2,2,2,2,4),(-11.8499565270215,
-11.8453602865149,-11.6442887880003,-11.4509185840308,-11.2497702173852,
-11.0563312257612,-10.8551076078354,-10.6616005804636,-10.4603032196308,
-10.2667289211856,-10.0653592228549,-9.87171842016381,-9.6702776922814,
-9.47657114566235,-9.27506060415086,-9.08131129636344,-8.87982706034636,
-8.68610284128992,-8.68543777224221),.UNSPECIFIED.);
#930=B_SPLINE_CURVE_WITH_KNOTS('',3,(#24107,#24108,#24109,#24110,#24111,
#24112,#24113,#24114,#24115,#24116,#24117,#24118,#24119,#24120,#24121,#24122,
#24123,#24124,#24125,#24126,#24127,#24128,#24129,#24130,#24131,#24132,#24133,
#24134,#24135,#24136,#24137,#24138,#24139,#24140,#24141,#24142),
 .UNSPECIFIED.,.F.,.F.,(4,2,2,2,2,2,2,2,2,2,2,2,2,2,2,2,2,4),(-32.3486283723407,
-32.2025269350576,-32.003894451693,-31.8119081627106,-31.6134241377314,
-31.4214349848199,-31.2231029659801,-31.0310991883577,-30.8329225394816,
-30.6408914676505,-30.4428733240406,-30.2508014446613,-30.0529446674791,
-29.8608177110558,-29.6631248415205,-29.4709278926409,-29.2734011069936,
-29.1971185456898),.UNSPECIFIED.);
#931=B_SPLINE_CURVE_WITH_KNOTS('',3,(#24147,#24148,#24149,#24150,#24151,
#24152,#24153,#24154,#24155,#24156,#24157,#24158,#24159,#24160,#24161,#24162,
#24163,#24164,#24165,#24166,#24167,#24168,#24169,#24170,#24171,#24172,#24173,
#24174,#24175,#24176,#24177,#24178,#24179,#24180,#24181,#24182),
 .UNSPECIFIED.,.F.,.F.,(4,2,2,2,2,2,2,2,2,2,2,2,2,2,2,2,2,4),(-15.009441259603,
-14.9953430620414,-14.7949594260182,-14.6021595264654,-14.4016815810857,
-14.2088094808993,-14.0082398828457,-13.8152955212959,-13.6146367850036,
-13.4216203037066,-13.2208748034208,-13.0277865097912,-12.8269564825509,
-12.633796817441,-12.4328843668124,-12.2396538761215,-12.0386609765248,
-11.8499565270215),.UNSPECIFIED.);
#932=B_SPLINE_CURVE_WITH_KNOTS('',3,(#24183,#24184,#24185,#24186,#24187,
#24188,#24189,#24190,#24191,#24192,#24193,#24194,#24195,#24196,#24197,#24198,
#24199,#24200,#24201,#24202,#24203,#24204,#24205,#24206,#24207,#24208,#24209,
#24210,#24211,#24212,#24213,#24214,#24215,#24216,#24217,#24218),
 .UNSPECIFIED.,.F.,.F.,(4,2,2,2,2,2,2,2,2,2,2,2,2,2,2,2,2,4),(-29.1971185456898,
-29.0811187359594,-28.883759802215,-28.6913762159564,-28.4941864535241,
-28.301685662787,-28.1046659060324,-27.9120319049695,-27.7151824717669,
-27.5223994253904,-27.3257200916267,-27.1327724566436,-26.9362624291837,
-26.7431351555522,-26.5467930764249,-26.3534719618308,-26.1572958989704,
-26.0460294638091),.UNSPECIFIED.);
#933=B_SPLINE_CURVE_WITH_KNOTS('',3,(#24223,#24224,#24225,#24226,#24227,
#24228,#24229,#24230,#24231,#24232,#24233,#24234,#24235,#24236,#24237,#24238,
#24239,#24240,#24241,#24242,#24243,#24244,#24245,#24246,#24247,#24248,#24249,
#24250,#24251,#24252,#24253,#24254,#24255,#24256,#24257,#24258),
 .UNSPECIFIED.,.F.,.F.,(4,2,2,2,2,2,2,2,2,2,2,2,2,2,2,2,2,4),(-18.1648534816952,
-18.1345623064237,-17.9350454383078,-17.7427812309514,-17.5431439069863,
-17.3508210506561,-17.1510669569855,-16.9586819589623,-16.7588146828344,
-16.5663646878438,-16.3663877041066,-16.1738704300427,-15.9737870904475,
-15.7812007653394,-15.5810142904072,-15.3883575917231,-15.1880710649215,
-15.009441259603),.UNSPECIFIED.);
#934=B_SPLINE_CURVE_WITH_KNOTS('',3,(#24259,#24260,#24261,#24262,#24263,
#24264,#24265,#24266,#24267,#24268,#24269,#24270,#24271,#24272,#24273,#24274,
#24275,#24276,#24277,#24278,#24279,#24280,#24281,#24282,#24283,#24284,#24285,
#24286,#24287,#24288,#24289,#24290,#24291,#24292,#24293,#24294),
 .UNSPECIFIED.,.F.,.F.,(4,2,2,2,2,2,2,2,2,2,2,2,2,2,2,2,2,4),(-26.0460294638091,
-25.9637676321335,-25.7677550828262,-25.5740073934036,-25.3781552970517,
-25.1841770843524,-24.9884818430204,-24.7942632805341,-24.5987207867594,
-24.4042534004878,-24.2088590716305,-24.0141357912462,-23.8188846094804,
-23.6238997923439,-23.4287863492596,-23.2335357782769,-23.0385543229855,
-22.894653858858),.UNSPECIFIED.);
#935=B_SPLINE_CURVE_WITH_KNOTS('',3,(#24299,#24300,#24301,#24302,#24303,
#24304,#24305,#24306,#24307,#24308,#24309,#24310,#24311,#24312,#24313,#24314,
#24315,#24316,#24317,#24318,#24319,#24320,#24321,#24322,#24323,#24324,#24325,
#24326,#24327,#24328,#24329,#24330,#24331,#24332,#24333,#24334),
 .UNSPECIFIED.,.F.,.F.,(4,2,2,2,2,2,2,2,2,2,2,2,2,2,2,2,2,4),(-21.3177166421035,
-21.2625812719389,-21.064165629947,-20.8721490272244,-20.673582562973,-20.4815649801061,
-20.2828512953899,-20.0908222560601,-19.8919650794903,-19.6999150834194,
-19.5009182308336,-19.3088387501402,-19.1097060879411,-18.9175895474012,
-18.7183249591171,-18.5261647028704,-18.3267720591113,-18.1648534816952),
 .UNSPECIFIED.);
#936=B_SPLINE_CURVE_WITH_KNOTS('',3,(#24335,#24336,#24337,#24338,#24339,
#24340,#24341,#24342,#24343,#24344,#24345,#24346,#24347,#24348,#24349,#24350,
#24351,#24352,#24353,#24354,#24355,#24356,#24357,#24358,#24359,#24360,#24361,
#24362,#24363,#24364,#24365,#24366,#24367,#24368,#24369,#24370),
 .UNSPECIFIED.,.F.,.F.,(4,2,2,2,2,2,2,2,2,2,2,2,2,2,2,2,2,4),(-22.894653858858,
-22.8430351800972,-22.6481796696925,-22.4523904874596,-22.2576546387054,
-22.0615952329455,-21.8669725741083,-21.6706439608552,-21.4761278826948,
-21.2795321828928,-21.0851159879305,-20.8882563232672,-20.6939332725896,
-20.4968136557196,-20.3025770127114,-20.1052022348834,-19.911045305434,
-19.7420141160744),.UNSPECIFIED.);
#937=B_SPLINE_CURVE_WITH_KNOTS('',3,(#24375,#24376,#24377,#24378,#24379,
#24380,#24381,#24382,#24383,#24384,#24385,#24386,#24387,#24388,#24389,#24390,
#24391,#24392,#24393,#24394,#24395,#24396,#24397,#24398,#24399,#24400,#24401,
#24402,#24403,#24404,#24405,#24406,#24407,#24408,#24409,#24410),
 .UNSPECIFIED.,.F.,.F.,(4,2,2,2,2,2,2,2,2,2,2,2,2,2,2,2,2,4),(-24.4694816405073,
-24.3817664053116,-24.184657336375,-23.9921690598734,-23.7948901903441,
-23.6025135998707,-23.4050659356891,-23.2127850875403,-23.0151701076872,
-22.8229693137646,-22.625188932334,-22.4330529221295,-22.2351094468282,
-22.0430235119941,-21.84491960015,-21.6528697189484,-21.4546083320897,-21.3177166421035),
 .UNSPECIFIED.);
#938=B_SPLINE_CURVE_WITH_KNOTS('',3,(#24411,#24412,#24413,#24414,#24415,
#24416,#24417,#24418,#24419,#24420,#24421,#24422,#24423,#24424,#24425,#24426,
#24427,#24428,#24429,#24430,#24431,#24432,#24433,#24434,#24435,#24436,#24437,
#24438,#24439,#24440,#24441,#24442,#24443,#24444,#24445,#24446),
 .UNSPECIFIED.,.F.,.F.,(4,2,2,2,2,2,2,2,2,2,2,2,2,2,2,2,2,4),(-19.7420141160744,
-19.7134208241997,-19.5193369930586,-19.3214688202648,-19.1217779356284,
-18.9294364317553,-18.7296310935017,-18.5372255598661,-18.3373092864661,
-18.1448372418786,-17.9448134301776,-17.7522729260411,-17.5521448443219,
-17.3595344029897,-17.1593051843462,-16.9666237403786,-16.7662963782371,
-16.5866685152428),.UNSPECIFIED.);
#939=B_SPLINE_CURVE_WITH_KNOTS('',3,(#24451,#24452,#24453,#24454,#24455,
#24456,#24457,#24458,#24459,#24460,#24461,#24462,#24463,#24464,#24465,#24466,
#24467,#24468,#24469,#24470,#24471,#24472,#24473,#24474,#24475,#24476,#24477,
#24478,#24479,#24480,#24481,#24482,#24483,#24484,#24485,#24486),
 .UNSPECIFIED.,.F.,.F.,(4,2,2,2,2,2,2,2,2,2,2,2,2,2,2,2,2,4),(-27.6210776549999,
-27.4991473095919,-27.3015146936668,-27.1092429712434,-26.9117774887184,
-26.7194116960812,-26.5221148737608,-26.3296390861027,-26.1325119815572,
-25.9399101751814,-25.7429533429172,-25.5502095797723,-25.353423042936,
-25.1605216602857,-24.9639048847822,-24.770830509061,-24.57438239134,-24.4694816405073),
 .UNSPECIFIED.);
#940=B_SPLINE_CURVE_WITH_KNOTS('',3,(#24487,#24488,#24489,#24490,#24491,
#24492,#24493,#24494,#24495,#24496,#24497,#24498,#24499,#24500,#24501,#24502,
#24503,#24504,#24505,#24506,#24507,#24508,#24509,#24510,#24511,#24512,#24513,
#24514,#24515,#24516,#24517,#24518,#24519,#24520,#24521,#24522),
 .UNSPECIFIED.,.F.,.F.,(4,2,2,2,2,2,2,2,2,2,2,2,2,2,2,2,2,4),(-16.5866685152428,
-16.5735432232291,-16.3731205687638,-16.1802953001972,-15.979780061394,
-15.7868825357782,-15.5862772779135,-15.39330756832,-15.1926147156369,-14.9995730736048,
-14.7987949119831,-14.6056817336746,-14.4048204141143,-14.2116362105224,
-14.0106937532715,-13.8174391242358,-13.6164174234198,-13.4271423741323),
 .UNSPECIFIED.);
#941=B_SPLINE_CURVE_WITH_KNOTS('',3,(#24527,#24528,#24529,#24530,#24531,
#24532,#24533,#24534,#24535,#24536,#24537,#24538,#24539,#24540,#24541,#24542,
#24543,#24544,#24545,#24546,#24547,#24548,#24549,#24550,#24551,#24552,#24553,
#24554,#24555,#24556,#24557,#24558,#24559,#24560,#24561,#24562),
 .UNSPECIFIED.,.F.,.F.,(4,2,2,2,2,2,2,2,2,2,2,2,2,2,2,2,2,4),(-30.7732540162916,
-30.6224625534038,-30.4235903739139,-30.2315594873663,-30.0328304001711,
-29.8408120197825,-29.6422297645305,-29.4502135167174,-29.2517817105492,
-29.0597562579787,-28.8614783536651,-28.6694314282219,-28.4713106702696,
-28.2792291277839,-28.0812685071763,-27.8891384048115,-27.6913406131706,
-27.6210776549999),.UNSPECIFIED.);
#942=B_SPLINE_CURVE_WITH_KNOTS('',3,(#24563,#24564,#24565,#24566,#24567,
#24568,#24569,#24570,#24571,#24572,#24573,#24574,#24575,#24576,#24577,#24578,
#24579,#24580,#24581,#24582,#24583,#24584,#24585,#24586,#24587,#24588,#24589,
#24590,#24591,#24592,#24593,#24594,#24595,#24596,#24597,#24598,#24599,#24600),
 .UNSPECIFIED.,.F.,.F.,(4,2,2,2,2,2,2,2,2,2,2,2,2,2,2,2,2,2,4),(-13.4271423741323,
-13.4230930351638,-13.2219938637853,-13.0286004296796,-12.827425444877,
-12.6339637091196,-12.4327144575865,-12.2391851814991,-12.0378631049865,
-11.8442670556327,-11.6428734964602,-11.4492114373098,-11.2477476438319,
-11.0540203272119,-10.8524874591921,-10.6587180709674,-10.457263865068,
-10.2635182555291,-10.262509796578),.UNSPECIFIED.);
#943=B_SPLINE_CURVE_WITH_KNOTS('',3,(#24605,#24606,#24607,#24608,#24609,
#24610,#24611,#24612,#24613,#24614,#24615,#24616,#24617,#24618,#24619,#24620,
#24621,#24622,#24623,#24624,#24625,#24626,#24627,#24628,#24629,#24630,#24631,
#24632,#24633,#24634,#24635,#24636,#24637,#24638,#24639,#24640),
 .UNSPECIFIED.,.F.,.F.,(4,2,2,2,2,2,2,2,2,2,2,2,2,2,2,2,2,4),(-33.9272264020338,
-33.7557592376309,-33.5558801431226,-33.3634883384545,-33.1637220538787,
-32.9713927215123,-32.7717428228324,-32.5794725404251,-32.3799427040667,
-32.1877273544111,-31.9883213410583,-31.7961560494673,-31.5968776846587,
-31.4047567598856,-31.2056099112557,-31.0135267921333,-30.814515343206,
-30.7732540162916),.UNSPECIFIED.);
#944=B_SPLINE_CURVE_WITH_KNOTS('',3,(#24641,#24642,#24643,#24644,#24645,
#24646,#24647,#24648,#24649,#24650,#24651,#24652,#24653,#24654,#24655,#24656,
#24657,#24658,#24659,#24660,#24661,#24662,#24663,#24664,#24665,#24666,#24667,
#24668,#24669,#24670,#24671,#24672,#24673,#24674,#24675,#24676),
 .UNSPECIFIED.,.F.,.F.,(4,2,2,2,2,2,2,2,2,2,2,2,2,2,2,2,2,4),(-10.262509796578,
-10.0621748049494,-9.86845075919977,-9.66722218278625,-9.47351732981415,
-9.27240799880696,-9.07871980290119,-8.87773434771368,-8.68406009983074,
-8.48320341539374,-8.28954022456674,-8.08881747388833,-7.89516225877231,
-7.69457887431953,-7.5009283550059,-7.30049003747721,-7.10684072770255,
-7.09973172643055),.UNSPECIFIED.);
#945=B_SPLINE_CURVE_WITH_KNOTS('',3,(#24681,#24682,#24683,#24684,#24685,
#24686,#24687,#24688,#24689,#24690,#24691,#24692,#24693,#24694,#24695,#24696,
#24697,#24698,#24699,#24700,#24701,#24702,#24703,#24704,#24705,#24706,#24707,
#24708,#24709,#24710,#24711,#24712,#24713,#24714,#24715,#24716),
 .UNSPECIFIED.,.F.,.F.,(4,2,2,2,2,2,2,2,2,2,2,2,2,2,2,2,2,4),(-37.0845565341341,
-36.9000799964494,-36.6994119173651,-36.5064598623789,-36.3058806641965,
-36.1130008645257,-35.9125130467586,-35.719705464902,-35.5193116691429,
-35.3265760288943,-35.1262790398785,-34.9336147815065,-34.7334175268641,
-34.540823757936,-34.3407293064061,-34.1482047484434,-33.948216306308,-33.9272264020338),
 .UNSPECIFIED.);
#946=B_SPLINE_CURVE_WITH_KNOTS('',3,(#24717,#24718,#24719,#24720,#24721,
#24722,#24723,#24724,#24725,#24726,#24727,#24728,#24729,#24730,#24731,#24732,
#24733,#24734,#24735,#24736,#24737,#24738,#24739,#24740,#24741,#24742,#24743,
#24744,#24745,#24746,#24747,#24748,#24749,#24750,#24751,#24752),
 .UNSPECIFIED.,.F.,.F.,(4,2,2,2,2,2,2,2,2,2,2,2,2,2,2,2,2,4),(-7.09973172643055,
-6.90655344170533,-6.71290164162491,-6.51277160774573,-6.31911339745019,
-6.11914708016145,-5.92547831414216,-5.72568240496176,-5.53199870774885,
-5.33238010304901,-5.13867686627481,-4.93924263913638,-4.74551502028898,
-4.54627238580402,-4.3525153089586,-4.15347158241934,-3.9596797412452,-3.94188496449128),
 .UNSPECIFIED.);
#947=B_SPLINE_CURVE_WITH_KNOTS('',3,(#24757,#24758,#24759,#24760,#24761,
#24762,#24763,#24764,#24765,#24766,#24767,#24768,#24769,#24770,#24771,#24772,
#24773,#24774,#24775,#24776,#24777,#24778,#24779,#24780,#24781,#24782,#24783,
#24784,#24785,#24786,#24787,#24788,#24789,#24790,#24791,#24792),
 .UNSPECIFIED.,.F.,.F.,(4,2,2,2,2,2,2,2,2,2,2,2,2,2,2,2,2,4),(-40.2466139348711,
-40.0545403932037,-39.8532352583116,-39.6597210230983,-39.4584894779182,
-39.2650431981048,-39.063886739874,-38.8705091692816,-38.6694294031336,
-38.4761212714501,-38.2751199158824,-38.0818819135985,-37.8809608058188,
-37.687793566387,-37.4869546674465,-37.2938587463589,-37.0931041459699,
-37.0845565341341),.UNSPECIFIED.);
#948=B_SPLINE_CURVE_WITH_KNOTS('',3,(#24793,#24794,#24795,#24796,#24797,
#24798,#24799,#24800,#24801,#24802,#24803,#24804,#24805,#24806,#24807,#24808,
#24809,#24810,#24811,#24812,#24813,#24814,#24815,#24816,#24817,#24818,#24819,
#24820,#24821,#24822,#24823,#24824,#24825,#24826,#24827,#24828),
 .UNSPECIFIED.,.F.,.F.,(4,2,2,2,2,2,2,2,2,2,2,2,2,2,2,2,2,4),(-3.94188496449128,
-3.76084228872693,-3.56701015207919,-3.36838633300804,-3.17450815341289,
-2.97610525484641,-2.7821750801714,-2.58400024268388,-2.39001193128194,
-2.19207206656769,-1.99801930613313,-1.80032100669122,-1.60619733703843,
-1.40874677861415,-1.21454561850871,-1.01734845629544,-0.823063134397515,
-0.787742139522384),.UNSPECIFIED.);
#949=B_SPLINE_CURVE_WITH_KNOTS('',3,(#24831,#24832,#24833,#24834,#24835,
#24836,#24837,#24838,#24839,#24840,#24841,#24842),.UNSPECIFIED.,.F.,.F.,
(4,2,2,2,2,4),(-0.787742139522384,-0.626124599551191,-0.43174863618738,
-0.235072853109506,-0.116437106936023,-9.99999992812306E-7),
 .UNSPECIFIED.);
#950=B_SPLINE_CURVE_WITH_KNOTS('',3,(#24845,#24846,#24847,#24848,#24849,
#24850,#24851,#24852),.UNSPECIFIED.,.F.,.F.,(4,2,2,4),(-40.6422236169032,
-40.4452026475075,-40.2481218184496,-40.2466139348711),.UNSPECIFIED.);
#951=B_SPLINE_CURVE_WITH_KNOTS('',3,(#24879,#24880,#24881,#24882,#24883,
#24884,#24885,#24886,#24887,#24888,#24889,#24890),.UNSPECIFIED.,.F.,.F.,
(4,2,2,2,2,4),(-2.81763482151145,-2.66615582776095,-2.46478441849091,-2.19827513744825,
-1.9545528152173,-1.82223598960404),.UNSPECIFIED.);
#952=B_SPLINE_CURVE_WITH_KNOTS('',3,(#24895,#24896,#24897,#24898,#24899,
#24900,#24901,#24902,#24903,#24904,#24905,#24906,#24907,#24908,#24909,#24910,
#24911,#24912,#24913,#24914,#24915,#24916,#24917,#24918,#24919,#24920),
 .UNSPECIFIED.,.F.,.F.,(4,2,2,2,2,2,2,2,2,2,2,2,4),(-1.82223598960404,-1.7229258160528,
-1.51102009351715,-1.30997005387127,-1.21842619461754,-1.04088214590786,
-0.861129971477336,-0.676603178308848,-0.585954297377947,-0.411830214191357,
-0.231403986438724,-0.115329226334212,0.),.UNSPECIFIED.);
#953=B_SPLINE_CURVE_WITH_KNOTS('',3,(#24923,#24924,#24925,#24926,#24927,
#24928,#24929,#24930,#24931,#24932,#24933,#24934),.UNSPECIFIED.,.F.,.F.,
(4,2,2,2,2,4),(-0.353981642318911,-0.271813414514787,-0.183870482640077,
-0.100406136832525,-0.0580770708076673,0.),.UNSPECIFIED.);
#954=B_SPLINE_CURVE_WITH_KNOTS('',3,(#26251,#26252,#26253,#26254,#26255,
#26256,#26257,#26258,#26259,#26260,#26261,#26262,#26263,#26264,#26265,#26266,
#26267,#26268),.UNSPECIFIED.,.F.,.F.,(4,2,2,2,2,2,2,2,4),(23.6688063208097,
23.8680016439259,24.0616943144381,24.2627278650596,24.4564054848417,24.6573122520947,
24.8509776384353,25.0517525666804,25.2503481109993),.UNSPECIFIED.);
#955=B_SPLINE_CURVE_WITH_KNOTS('',3,(#26272,#26273,#26274,#26275,#26276,
#26277,#26278,#26279,#26280,#26281,#26282,#26283,#26284,#26285,#26286,#26287,
#26288,#26289,#26290,#26291),.UNSPECIFIED.,.F.,.F.,(4,2,2,2,2,2,2,2,2,4),
(0.,0.192309890628632,0.392950131878038,0.585822092254251,0.786391070426237,
0.979196478715363,1.17969285299266,1.37243094502364,1.57285327532948,1.5761150882838),
 .UNSPECIFIED.);
#956=B_SPLINE_CURVE_WITH_KNOTS('',3,(#26295,#26296,#26297,#26298,#26299,
#26300,#26301,#26302,#26303,#26304,#26305,#26306,#26307,#26308,#26309,#26310,
#26311,#26312,#26313,#26314,#26315,#26316,#26317,#26318,#26319,#26320,#26321,
#26322,#26323,#26324,#26325,#26326,#26327,#26328,#26329,#26330),
 .UNSPECIFIED.,.F.,.F.,(4,2,2,2,2,2,2,2,2,2,2,2,2,2,2,2,2,4),(1.5761150882838,
1.76552329302677,1.96587003453306,2.15847123733424,2.35874073498249,2.55127241358088,
2.75146289668655,2.94392438938976,3.1440339664105,3.33642467841756,3.53645133198428,
3.72877075788602,3.92871234020673,4.12096009000703,4.32081431877349,4.51299014771225,
4.71275460265744,4.72444996915763),.UNSPECIFIED.);
#957=B_SPLINE_CURVE_WITH_KNOTS('',3,(#26335,#26336,#26337,#26338,#26339,
#26340,#26341,#26342,#26343,#26344,#26345,#26346,#26347,#26348,#26349,#26350,
#26351,#26352,#26353,#26354,#26355,#26356,#26357,#26358,#26359,#26360,#26361,
#26362,#26363,#26364,#26365,#26366,#26367,#26368,#26369,#26370,#26371,#26372),
 .UNSPECIFIED.,.F.,.F.,(4,2,2,2,2,2,2,2,2,2,2,2,2,2,2,2,2,2,4),(20.5033787905061,
20.506181756931,20.707436476315,20.9009725341327,21.1023006757468,21.2959038362448,
21.4973040170517,21.6909735141241,21.8924444473212,22.0861795230845,22.2877200126867,
22.4814976181688,22.6829930094403,22.8767459939412,23.0781322065223,23.2718627249666,
23.4731357386561,23.6668460986838,23.6688063208097),.UNSPECIFIED.);
#958=B_SPLINE_CURVE_WITH_KNOTS('',3,(#26373,#26374,#26375,#26376,#26377,
#26378,#26379,#26380,#26381,#26382,#26383,#26384,#26385,#26386,#26387,#26388,
#26389,#26390,#26391,#26392,#26393,#26394,#26395,#26396,#26397,#26398,#26399,
#26400,#26401,#26402,#26403,#26404,#26405,#26406,#26407,#26408),
 .UNSPECIFIED.,.F.,.F.,(4,2,2,2,2,2,2,2,2,2,2,2,2,2,2,2,2,4),(4.72444996915763,
4.90485844507989,5.10453056535011,5.2965625728159,5.49613965534028,5.68810023909005,
5.88757943815145,6.0794693159494,6.27884764417189,6.47066789141356,6.66994222240167,
6.86169432721906,7.06086140009344,7.25254732199799,7.4516037480787,7.64322597946192,
7.8421682513544,7.86845984801116),.UNSPECIFIED.);
#959=B_SPLINE_CURVE_WITH_KNOTS('',3,(#26413,#26414,#26415,#26416,#26417,
#26418,#26419,#26420,#26421,#26422,#26423,#26424,#26425,#26426,#26427,#26428,
#26429,#26430,#26431,#26432,#26433,#26434,#26435,#26436,#26437,#26438,#26439,
#26440,#26441,#26442,#26443,#26444,#26445,#26446,#26447,#26448),
 .UNSPECIFIED.,.F.,.F.,(4,2,2,2,2,2,2,2,2,2,2,2,2,2,2,2,2,4),(17.3423091084718,
17.3532026119064,17.5538068254068,17.7467812232279,17.9474740334127,18.1405205000154,
18.341299563721,18.5344177588769,18.7352808693728,18.9284703261504,19.1294154092585,
19.3226755615564,19.5237006712113,19.7170308776452,19.9181341910316,20.1115337554729,
20.3127135678619,20.5033787905061),.UNSPECIFIED.);
#960=B_SPLINE_CURVE_WITH_KNOTS('',3,(#26449,#26450,#26451,#26452,#26453,
#26454,#26455,#26456,#26457,#26458,#26459,#26460,#26461,#26462,#26463,#26464,
#26465,#26466,#26467,#26468,#26469,#26470,#26471,#26472,#26473,#26474,#26475,
#26476,#26477,#26478,#26479,#26480,#26481,#26482,#26483,#26484),
 .UNSPECIFIED.,.F.,.F.,(4,2,2,2,2,2,2,2,2,2,2,2,2,2,2,2,2,4),(7.86845984801116,
8.03372988091695,8.23255438425071,8.4240591611593,8.62276218921183,8.81421458649587,
9.00793068521309,9.20384682448228,9.39766192439471,9.59331213805431,9.78723291767305,
9.98261501021267,10.1766480638836,10.3717609328959,10.5659127218738,10.7607564538351,
10.9550332555806,11.0096450714467),.UNSPECIFIED.);
#961=B_SPLINE_CURVE_WITH_KNOTS('',3,(#26489,#26490,#26491,#26492,#26493,
#26494,#26495,#26496,#26497,#26498,#26499,#26500,#26501,#26502,#26503,#26504,
#26505,#26506,#26507,#26508,#26509,#26510,#26511,#26512,#26513,#26514,#26515,
#26516,#26517,#26518,#26519,#26520,#26521,#26522,#26523,#26524),
 .UNSPECIFIED.,.F.,.F.,(4,2,2,2,2,2,2,2,2,2,2,2,2,2,2,2,2,4),(14.1856813666801,
14.2106556084505,14.4104497800149,14.602862920382,14.8027694881212,14.9952481928414,
15.1952637085973,15.387810139388,15.5879312801588,15.7805471024998,15.9807706780298,
16.1734571212125,16.3737800793295,16.5665379931835,16.7669574231372,16.9597873308951,
17.1603004649466,17.3423091084718),.UNSPECIFIED.);
#962=B_SPLINE_CURVE_WITH_KNOTS('',3,(#26525,#26526,#26527,#26528,#26529,
#26530,#26531,#26532,#26533,#26534,#26535,#26536,#26537,#26538,#26539,#26540,
#26541,#26542,#26543,#26544,#26545,#26546,#26547,#26548,#26549,#26550,#26551,
#26552,#26553,#26554,#26555,#26556,#26557,#26558,#26559,#26560),
 .UNSPECIFIED.,.F.,.F.,(4,2,2,2,2,2,2,2,2,2,2,2,2,2,2,2,2,4),(11.0096450714467,
11.1496092096788,11.3440170662402,11.5383279428451,11.7328726093068,11.926922499806,
12.1216093938707,12.3154038088951,12.5102379627232,12.7037838362626,12.8987698517158,
13.0920755192803,13.287217527673,13.4802926774533,13.6755943048501,13.8684499017687,
14.0639142407318,14.1497226382099),.UNSPECIFIED.);
#963=B_SPLINE_CURVE_WITH_KNOTS('',3,(#26565,#26566,#26567,#26568,#26569,
#26570,#26571,#26572,#26573,#26574,#26575,#26576,#26577,#26578,#26579,#26580,
#26581,#26582,#26583,#26584,#26585,#26586,#26587,#26588,#26589,#26590,#26591,
#26592,#26593,#26594,#26595,#26596,#26597,#26598,#26599,#26600),
 .UNSPECIFIED.,.F.,.F.,(4,2,2,2,2,2,2,2,2,2,2,2,2,2,2,2,2,4),(11.032043594273,
11.0791330610422,11.2738662174345,11.470065184074,11.6646875517819,11.8611551219302,
12.0601971336175,12.2522980304616,12.4514749854863,12.6436145256115,12.8429225405824,
13.0351071786466,13.2345423893918,13.4267777160951,13.6263363034536,13.8186270997122,
14.0183053118855,14.1856813666801),.UNSPECIFIED.);
#964=B_SPLINE_CURVE_WITH_KNOTS('',3,(#26601,#26602,#26603,#26604,#26605,
#26606,#26607,#26608,#26609,#26610,#26611,#26612,#26613,#26614,#26615,#26616,
#26617,#26618,#26619,#26620,#26621,#26622,#26623,#26624,#26625,#26626,#26627,
#26628,#26629,#26630,#26631,#26632,#26633,#26634,#26635,#26636),
 .UNSPECIFIED.,.F.,.F.,(4,2,2,2,2,2,2,2,2,2,2,2,2,2,2,2,2,4),(14.1497226382099,
14.2565624242763,14.452192012803,14.644645970566,14.8404427787485,15.0327165985864,
15.2286820237912,15.4207906366718,15.6169255143855,15.8088843871035,16.0051889839162,
16.1970138736636,16.3934879143908,16.5851947634573,16.7818374560417,16.9734422046251,
17.1702522710418,17.2895966666142),.UNSPECIFIED.);
#965=B_SPLINE_CURVE_WITH_KNOTS('',3,(#26641,#26642,#26643,#26644,#26645,
#26646,#26647,#26648,#26649,#26650,#26651,#26652,#26653,#26654,#26655,#26656,
#26657,#26658,#26659,#26660,#26661,#26662,#26663,#26664,#26665,#26666,#26667,
#26668,#26669,#26670,#26671,#26672,#26673,#26674,#26675,#26676),
 .UNSPECIFIED.,.F.,.F.,(4,2,2,2,2,2,2,2,2,2,2,2,2,2,2,2,2,4),(7.8798925984307,
7.95653091972942,8.1523647619255,8.34647021357625,8.54214862603429,8.73649776288571,
8.93202503348979,9.12662581805227,9.32200669581487,9.51686567465596,9.71210532789297,
9.90722761742384,10.1023315877192,10.2977208855736,10.4926950386617,10.6883536586088,
10.8832041333213,11.032043594273),.UNSPECIFIED.);
#966=B_SPLINE_CURVE_WITH_KNOTS('',3,(#26677,#26678,#26679,#26680,#26681,
#26682,#26683,#26684,#26685,#26686,#26687,#26688,#26689,#26690,#26691,#26692,
#26693,#26694,#26695,#26696,#26697,#26698,#26699,#26700,#26701,#26702,#26703,
#26704,#26705,#26706,#26707,#26708,#26709,#26710,#26711,#26712),
 .UNSPECIFIED.,.F.,.F.,(4,2,2,2,2,2,2,2,2,2,2,2,2,2,2,2,2,4),(17.2895966666142,
17.3617706775084,17.5587463897173,17.7501938628928,17.9473330828076,18.1387245302062,
18.336024752601,18.527374447667,18.7248328449502,18.9161543154852,19.1137677833141,
19.3050737223178,19.5028389250998,19.6941411243536,19.8920545397888,20.0833638456821,
20.2814218076159,20.4299877360611),.UNSPECIFIED.);
#967=B_SPLINE_CURVE_WITH_KNOTS('',3,(#26717,#26718,#26719,#26720,#26721,
#26722,#26723,#26724,#26725,#26726,#26727,#26728,#26729,#26730,#26731,#26732,
#26733,#26734,#26735,#26736,#26737,#26738,#26739,#26740,#26741,#26742,#26743,
#26744,#26745,#26746,#26747,#26748,#26749,#26750,#26751,#26752),
 .UNSPECIFIED.,.F.,.F.,(4,2,2,2,2,2,2,2,2,2,2,2,2,2,2,2,2,4),(4.72815874405663,
4.8384872813078,5.03565472956953,5.22824215554031,5.42523938450227,5.61796591852915,
5.81479280753122,6.00767417677815,6.20433115727545,6.39738279865264,6.59387087295077,
6.78710752149101,6.98342825882622,7.17686380974204,7.37301935402876,7.56666675378859,
7.762659815928,7.8798925984307),.UNSPECIFIED.);
#968=B_SPLINE_CURVE_WITH_KNOTS('',3,(#26753,#26754,#26755,#26756,#26757,
#26758,#26759,#26760,#26761,#26762,#26763,#26764,#26765,#26766,#26767,#26768,
#26769,#26770,#26771,#26772,#26773,#26774,#26775,#26776,#26777,#26778,#26779,
#26780,#26781,#26782,#26783,#26784,#26785,#26786,#26787,#26788),
 .UNSPECIFIED.,.F.,.F.,(4,2,2,2,2,2,2,2,2,2,2,2,2,2,2,2,2,4),(20.4299877360611,
20.472748098005,20.6709468369917,20.8622990173113,21.0606346984189,21.2520207148496,
21.4504894723635,21.6419163395927,21.8405143083974,22.0319881493852,22.2307114929069,
22.4222375880747,22.621082522768,22.8126653661272,23.0116281825616,23.2032715424857,
23.4023486231547,23.5720713493618),.UNSPECIFIED.);
#969=B_SPLINE_CURVE_WITH_KNOTS('',3,(#26794,#26795,#26796,#26797,#26798,
#26799,#26800,#26801,#26802,#26803,#26804,#26805),.UNSPECIFIED.,.F.,.F.,
(4,2,2,2,2,4),(26.717398205925,26.7265409725364,26.9265040240299,27.1188444098408,
27.31889260268,27.5043317305357),.UNSPECIFIED.);
#970=B_SPLINE_CURVE_WITH_KNOTS('',3,(#26808,#26809,#26810,#26811,#26812,
#26813,#26814,#26815,#26816,#26817,#26818,#26819,#26820,#26821,#26822,#26823,
#26824,#26825,#26826,#26827),.UNSPECIFIED.,.F.,.F.,(4,2,2,2,2,2,2,2,2,4),
(0.,0.175931162978202,0.353160743648948,0.545227872409306,0.74413522592968,
0.936178861517958,1.13494379915102,1.32697316334426,1.52559192745073,1.57613829627577),
 .UNSPECIFIED.);
#971=B_SPLINE_CURVE_WITH_KNOTS('',3,(#26829,#26830,#26831,#26832,#26833,
#26834,#26835,#26836,#26837,#26838,#26839,#26840,#26841,#26842,#26843,#26844,
#26845,#26846,#26847,#26848,#26849,#26850,#26851,#26852,#26853,#26854,#26855,
#26856,#26857,#26858,#26859,#26860,#26861,#26862,#26863,#26864),
 .UNSPECIFIED.,.F.,.F.,(4,2,2,2,2,2,2,2,2,2,2,2,2,2,2,2,2,4),(1.57613829627577,
1.71761721885756,1.91608616703187,2.10811855179259,2.30643419830044,2.4984857808909,
2.69664484024402,2.88872861275038,3.08672804477878,3.27885781362127,3.47669486927162,
3.6688851591046,3.86655742608426,4.05882336145931,4.25632880874467,4.44868597504655,
4.64602299520801,4.72815874405663),.UNSPECIFIED.);
#972=B_SPLINE_CURVE_WITH_KNOTS('',3,(#26865,#26866,#26867,#26868,#26869,
#26870,#26871,#26872,#26873,#26874,#26875,#26876,#26877,#26878,#26879,#26880,
#26881,#26882,#26883,#26884,#26885,#26886,#26887,#26888,#26889,#26890,#26891,
#26892,#26893,#26894,#26895,#26896,#26897,#26898,#26899,#26900),
 .UNSPECIFIED.,.F.,.F.,(4,2,2,2,2,2,2,2,2,2,2,2,2,2,2,2,2,4),(23.5720713493618,
23.5940556057397,23.7932434397696,23.9850165529989,24.184311747963,24.3761529651803,
24.5755522562542,24.767463077738,24.9669633344463,25.1589448461464,25.3585430769529,
25.550596005705,25.7502893607003,25.9424141254523,26.1421998973837,26.3343966561616,
26.5342722800385,26.717398205925),.UNSPECIFIED.);
#973=B_SPLINE_CURVE_WITH_KNOTS('',3,(#26932,#26933,#26934,#26935,#26936,
#26937,#26938,#26939,#26940,#26941,#26942,#26943,#26944,#26945),
 .UNSPECIFIED.,.F.,.F.,(4,2,2,2,2,2,4),(-1.09561114978705,-0.811392982779186,
-0.600348101262501,-0.377067356850475,-0.216075223113698,-0.119074012181648,
0.),.UNSPECIFIED.);
#974=B_SPLINE_CURVE_WITH_KNOTS('',3,(#26946,#26947,#26948,#26949,#26950,
#26951,#26952,#26953,#26954,#26955,#26956,#26957,#26958,#26959),
 .UNSPECIFIED.,.F.,.F.,(4,2,2,2,2,2,4),(-0.920708721485626,-0.810769067465036,
-0.701870911977783,-0.530236332505368,-0.314467713567416,-0.153407050270327,
0.),.UNSPECIFIED.);
#975=CYLINDRICAL_SURFACE('',#12318,4.5);
#976=CYLINDRICAL_SURFACE('',#12373,4.);
#977=CYLINDRICAL_SURFACE('',#12383,6.00000000000001);
#978=CYLINDRICAL_SURFACE('',#12386,13.);
#979=CYLINDRICAL_SURFACE('',#12387,13.);
#980=CYLINDRICAL_SURFACE('',#12388,16.);
#981=CYLINDRICAL_SURFACE('',#12389,27.);
#982=CYLINDRICAL_SURFACE('',#12391,9.50000000000001);
#983=CYLINDRICAL_SURFACE('',#12393,5.99999999999999);
#984=CYLINDRICAL_SURFACE('',#12396,8.00000000000001);
#985=CYLINDRICAL_SURFACE('',#12399,7.99999999999999);
#986=CYLINDRICAL_SURFACE('',#12402,13.);
#987=CYLINDRICAL_SURFACE('',#12403,13.);
#988=CYLINDRICAL_SURFACE('',#12404,16.);
#989=CYLINDRICAL_SURFACE('',#12405,9.50000000000001);
#990=CYLINDRICAL_SURFACE('',#12407,5.99999999999999);
#991=CYLINDRICAL_SURFACE('',#12410,8.00000000000001);
#992=CYLINDRICAL_SURFACE('',#12413,7.99999999999999);
#993=CYLINDRICAL_SURFACE('',#12416,9.50000000000001);
#994=CYLINDRICAL_SURFACE('',#12417,5.);
#995=CYLINDRICAL_SURFACE('',#12420,30.);
#996=CYLINDRICAL_SURFACE('',#12422,5.);
#997=CYLINDRICAL_SURFACE('',#12434,100.);
#998=CYLINDRICAL_SURFACE('',#12445,10.);
#999=CYLINDRICAL_SURFACE('',#12448,10.);
#1000=CYLINDRICAL_SURFACE('',#12479,10.);
#1001=CYLINDRICAL_SURFACE('',#12500,30.);
#1002=CYLINDRICAL_SURFACE('',#12509,10.);
#1003=CYLINDRICAL_SURFACE('',#12517,27.);
#1004=CYLINDRICAL_SURFACE('',#12522,100.);
#1005=CYLINDRICAL_SURFACE('',#12525,15.);
#1006=CYLINDRICAL_SURFACE('',#12526,15.);
#1007=CYLINDRICAL_SURFACE('',#12527,15.);
#1008=CYLINDRICAL_SURFACE('',#12528,15.);
#1009=CYLINDRICAL_SURFACE('',#12567,15.);
#1010=CYLINDRICAL_SURFACE('',#12568,15.);
#1011=CYLINDRICAL_SURFACE('',#12569,15.);
#1012=CYLINDRICAL_SURFACE('',#12570,15.);
#1013=CYLINDRICAL_SURFACE('',#12602,53.);
#1014=CYLINDRICAL_SURFACE('',#12603,53.);
#1015=CYLINDRICAL_SURFACE('',#12604,53.);
#1016=CYLINDRICAL_SURFACE('',#12605,53.);
#1017=CYLINDRICAL_SURFACE('',#12606,4.);
#1018=CYLINDRICAL_SURFACE('',#12608,4.);
#1019=CYLINDRICAL_SURFACE('',#12609,4.00000000000001);
#1020=CYLINDRICAL_SURFACE('',#12610,4.);
#1021=CYLINDRICAL_SURFACE('',#12612,4.);
#1022=CYLINDRICAL_SURFACE('',#12614,3.99999999999998);
#1023=CYLINDRICAL_SURFACE('',#12621,4.);
#1024=CYLINDRICAL_SURFACE('',#12623,4.);
#1025=CYLINDRICAL_SURFACE('',#12626,4.);
#1026=CYLINDRICAL_SURFACE('',#12627,4.);
#1027=CYLINDRICAL_SURFACE('',#12628,2.);
#1028=CYLINDRICAL_SURFACE('',#12629,2.);
#1029=CYLINDRICAL_SURFACE('',#12630,2.);
#1030=CYLINDRICAL_SURFACE('',#12631,2.);
#1031=CYLINDRICAL_SURFACE('',#12632,1.99999999999999);
#1032=CYLINDRICAL_SURFACE('',#12633,1.99999999999999);
#1033=CYLINDRICAL_SURFACE('',#12634,2.);
#1034=CYLINDRICAL_SURFACE('',#12635,2.);
#1035=CYLINDRICAL_SURFACE('',#12636,6.00000000000001);
#1036=CYLINDRICAL_SURFACE('',#12637,5.99999999999999);
#1037=CYLINDRICAL_SURFACE('',#12638,6.00000000000001);
#1038=CYLINDRICAL_SURFACE('',#12642,5.99999999999999);
#1039=CYLINDRICAL_SURFACE('',#12643,2.);
#1040=CYLINDRICAL_SURFACE('',#12644,2.);
#1041=CYLINDRICAL_SURFACE('',#12645,2.);
#1042=CYLINDRICAL_SURFACE('',#12646,2.);
#1043=CYLINDRICAL_SURFACE('',#12647,4.5);
#1044=CYLINDRICAL_SURFACE('',#12648,4.5);
#1045=CYLINDRICAL_SURFACE('',#12649,4.5);
#1046=CYLINDRICAL_SURFACE('',#12650,6.50000000000001);
#1047=CYLINDRICAL_SURFACE('',#12651,6.50000000000001);
#1048=CYLINDRICAL_SURFACE('',#12654,22.5);
#1049=CYLINDRICAL_SURFACE('',#12666,22.5);
#1050=CYLINDRICAL_SURFACE('',#12679,55.);
#1051=CYLINDRICAL_SURFACE('',#12682,55.);
#1052=CYLINDRICAL_SURFACE('',#12707,11.);
#1053=CYLINDRICAL_SURFACE('',#12708,7.99999999999999);
#1054=CYLINDRICAL_SURFACE('',#12709,7.99999999999999);
#1055=CYLINDRICAL_SURFACE('',#12711,15.);
#1056=CYLINDRICAL_SURFACE('',#12713,11.);
#1057=CYLINDRICAL_SURFACE('',#12715,7.99999999999999);
#1058=CYLINDRICAL_SURFACE('',#12717,7.99999999999999);
#1059=CYLINDRICAL_SURFACE('',#12720,15.);
#1060=CYLINDRICAL_SURFACE('',#12722,30.);
#1061=CYLINDRICAL_SURFACE('',#12724,7.99999999999999);
#1062=CYLINDRICAL_SURFACE('',#12737,25.);
#1063=CYLINDRICAL_SURFACE('',#12738,25.);
#1064=CYLINDRICAL_SURFACE('',#12745,5.);
#1065=CYLINDRICAL_SURFACE('',#12746,5.);
#1066=CYLINDRICAL_SURFACE('',#12747,2.);
#1067=CYLINDRICAL_SURFACE('',#12748,2.);
#1068=CYLINDRICAL_SURFACE('',#12760,7.89999999999999);
#1069=CYLINDRICAL_SURFACE('',#12762,13.);
#1070=CYLINDRICAL_SURFACE('',#12776,7.89999999999999);
#1071=CYLINDRICAL_SURFACE('',#12778,13.);
#1072=CYLINDRICAL_SURFACE('',#12827,12.5);
#1073=CYLINDRICAL_SURFACE('',#12873,13.);
#1074=CYLINDRICAL_SURFACE('',#12874,12.5);
#1075=CYLINDRICAL_SURFACE('',#12877,18.);
#1076=CYLINDRICAL_SURFACE('',#12881,13.5);
#1077=CYLINDRICAL_SURFACE('',#12884,13.5);
#1078=CYLINDRICAL_SURFACE('',#12886,8.00000000000002);
#1079=CYLINDRICAL_SURFACE('',#12889,8.00000000000002);
#1080=CYLINDRICAL_SURFACE('',#12892,15.);
#1081=CYLINDRICAL_SURFACE('',#12895,8.00000000000002);
#1082=CYLINDRICAL_SURFACE('',#12898,15.);
#1083=CYLINDRICAL_SURFACE('',#12901,3.);
#1084=CYLINDRICAL_SURFACE('',#12905,3.);
#1085=CYLINDRICAL_SURFACE('',#12925,8.00000000000001);
#1086=CYLINDRICAL_SURFACE('',#12926,8.00000000000001);
#1087=CYLINDRICAL_SURFACE('',#12940,20.);
#1088=CYLINDRICAL_SURFACE('',#12941,20.);
#1089=CYLINDRICAL_SURFACE('',#12942,20.);
#1090=CYLINDRICAL_SURFACE('',#12943,20.);
#1091=CYLINDRICAL_SURFACE('',#12952,8.00000000000001);
#1092=CYLINDRICAL_SURFACE('',#12962,8.);
#1093=CYLINDRICAL_SURFACE('',#12969,8.00000000000002);
#1094=CYLINDRICAL_SURFACE('',#12972,8.00000000000001);
#1095=CYLINDRICAL_SURFACE('',#12989,10.);
#1096=CYLINDRICAL_SURFACE('',#12990,9.99999999999999);
#1097=CYLINDRICAL_SURFACE('',#12991,10.);
#1098=CYLINDRICAL_SURFACE('',#12992,10.);
#1099=CYLINDRICAL_SURFACE('',#12995,0.5);
#1100=CYLINDRICAL_SURFACE('',#13007,7.50000000000001);
#1101=CYLINDRICAL_SURFACE('',#13010,5.);
#1102=CYLINDRICAL_SURFACE('',#13013,4.25);
#1103=CYLINDRICAL_SURFACE('',#13016,8.00000000000001);
#1104=CYLINDRICAL_SURFACE('',#13019,10.);
#1105=CYLINDRICAL_SURFACE('',#13025,10.);
#1106=CYLINDRICAL_SURFACE('',#13031,7.50000000000001);
#1107=CYLINDRICAL_SURFACE('',#13039,10.);
#1108=CYLINDRICAL_SURFACE('',#13042,23.);
#1109=CYLINDRICAL_SURFACE('',#13045,23.5);
#1110=CYLINDRICAL_SURFACE('',#13048,25.);
#1111=CYLINDRICAL_SURFACE('',#13051,27.);
#1112=CYLINDRICAL_SURFACE('',#13063,13.5);
#1113=CYLINDRICAL_SURFACE('',#13065,7.75000000000001);
#1114=CYLINDRICAL_SURFACE('',#13128,10.);
#1115=CYLINDRICAL_SURFACE('',#13130,10.);
#1116=CYLINDRICAL_SURFACE('',#13131,10.);
#1117=CYLINDRICAL_SURFACE('',#13133,10.);
#1118=CYLINDRICAL_SURFACE('',#13134,23.);
#1119=CYLINDRICAL_SURFACE('',#13135,23.);
#1120=CYLINDRICAL_SURFACE('',#13138,2.);
#1121=CYLINDRICAL_SURFACE('',#13142,2.);
#1122=CYLINDRICAL_SURFACE('',#13144,2.);
#1123=CYLINDRICAL_SURFACE('',#13146,1.99999999999999);
#1124=CYLINDRICAL_SURFACE('',#13148,2.);
#1125=CYLINDRICAL_SURFACE('',#13151,1.);
#1126=CYLINDRICAL_SURFACE('',#13154,0.999999999999998);
#1127=CYLINDRICAL_SURFACE('',#13156,1.00000000000001);
#1128=CYLINDRICAL_SURFACE('',#13158,0.999999999999998);
#1129=CYLINDRICAL_SURFACE('',#13160,1.00000000000001);
#1130=CYLINDRICAL_SURFACE('',#13162,1.);
#1131=CYLINDRICAL_SURFACE('',#13163,3.00000000000001);
#1132=CYLINDRICAL_SURFACE('',#13170,9.00000000000001);
#1133=CYLINDRICAL_SURFACE('',#13172,9.00000000000001);
#1134=CYLINDRICAL_SURFACE('',#13179,7.50000000000001);
#1135=CYLINDRICAL_SURFACE('',#13181,14.);
#1136=CYLINDRICAL_SURFACE('',#13187,3.99999999999999);
#1137=CYLINDRICAL_SURFACE('',#13190,2.99999999999999);
#1138=CYLINDRICAL_SURFACE('',#13193,4.00000000000004);
#1139=CYLINDRICAL_SURFACE('',#13196,2.99999999999999);
#1140=CYLINDRICAL_SURFACE('',#13199,4.00000000000004);
#1141=CYLINDRICAL_SURFACE('',#13235,3.49999999999998);
#1142=CYLINDRICAL_SURFACE('',#13237,5.50000000000002);
#1143=CYLINDRICAL_SURFACE('',#13239,5.50000000000002);
#1144=CYLINDRICAL_SURFACE('',#13241,3.49999999999998);
#1145=CYLINDRICAL_SURFACE('',#13244,1.99999999999999);
#1146=CYLINDRICAL_SURFACE('',#13246,3.99999999999998);
#1147=CYLINDRICAL_SURFACE('',#13248,3.99999999999998);
#1148=CYLINDRICAL_SURFACE('',#13250,1.99999999999999);
#1149=CYLINDRICAL_SURFACE('',#13254,3.37500000000002);
#1150=CYLINDRICAL_SURFACE('',#13257,3.37500000000002);
#1151=CYLINDRICAL_SURFACE('',#13264,1.);
#1152=CYLINDRICAL_SURFACE('',#13269,4.);
#1153=CYLINDRICAL_SURFACE('',#13274,6.99999999999999);
#1154=CYLINDRICAL_SURFACE('',#13283,1.);
#1155=CYLINDRICAL_SURFACE('',#13288,4.00000000000001);
#1156=CYLINDRICAL_SURFACE('',#13293,7.);
#1157=CYLINDRICAL_SURFACE('',#13319,0.999999999999997);
#1158=CYLINDRICAL_SURFACE('',#13322,0.999999999999983);
#1159=CYLINDRICAL_SURFACE('',#13325,0.999999999999997);
#1160=CYLINDRICAL_SURFACE('',#13328,1.00000000000002);
#1161=CYLINDRICAL_SURFACE('',#13331,1.00000000000002);
#1162=CYLINDRICAL_SURFACE('',#13348,1.);
#1163=CYLINDRICAL_SURFACE('',#13351,0.999999999999989);
#1164=CYLINDRICAL_SURFACE('',#13354,1.);
#1165=CYLINDRICAL_SURFACE('',#13357,0.999999999999999);
#1166=CYLINDRICAL_SURFACE('',#13360,0.999999999999993);
#1167=CYLINDRICAL_SURFACE('',#13370,4.50000000000001);
#1168=CYLINDRICAL_SURFACE('',#13373,4.99999999999999);
#1169=CYLINDRICAL_SURFACE('',#13376,4.50000000000001);
#1170=CYLINDRICAL_SURFACE('',#13379,4.99999999999999);
#1171=CYLINDRICAL_SURFACE('',#13382,10.);
#1172=CYLINDRICAL_SURFACE('',#13389,12.);
#1173=CYLINDRICAL_SURFACE('',#13414,27.);
#1174=CYLINDRICAL_SURFACE('',#13417,13.);
#1175=CYLINDRICAL_SURFACE('',#13429,12.);
#1176=CYLINDRICAL_SURFACE('',#13431,14.);
#1177=CYLINDRICAL_SURFACE('',#13445,24.);
#1178=CYLINDRICAL_SURFACE('',#13446,14.);
#1179=CYLINDRICAL_SURFACE('',#13464,6.);
#1180=CYLINDRICAL_SURFACE('',#13494,5.00000000000002);
#1181=CYLINDRICAL_SURFACE('',#13500,20.);
#1182=CYLINDRICAL_SURFACE('',#13504,20.);
#1183=CYLINDRICAL_SURFACE('',#13505,25.);
#1184=CYLINDRICAL_SURFACE('',#13542,5.00000000000001);
#1185=CYLINDRICAL_SURFACE('',#13548,20.);
#1186=CYLINDRICAL_SURFACE('',#13552,20.);
#1187=CYLINDRICAL_SURFACE('',#13553,25.);
#1188=CYLINDRICAL_SURFACE('',#13567,4.90000000000001);
#1189=CYLINDRICAL_SURFACE('',#13570,4.45873412499923);
#1190=CYLINDRICAL_SURFACE('',#13571,4.45873412499923);
#1191=CYLINDRICAL_SURFACE('',#13572,4.45873412499923);
#1192=CYLINDRICAL_SURFACE('',#13573,4.45873412499923);
#1193=CYLINDRICAL_SURFACE('',#13574,4.45873412499923);
#1194=CYLINDRICAL_SURFACE('',#13575,4.45873412499923);
#1195=CYLINDRICAL_SURFACE('',#13576,4.45873412499923);
#1196=CYLINDRICAL_SURFACE('',#13577,4.45873412499923);
#1197=CYLINDRICAL_SURFACE('',#13578,4.45873412499923);
#1198=CYLINDRICAL_SURFACE('',#13579,4.45873412499923);
#1199=CYLINDRICAL_SURFACE('',#13580,4.45873412499923);
#1200=CYLINDRICAL_SURFACE('',#13581,4.45873412499923);
#1201=CYLINDRICAL_SURFACE('',#13582,4.45873412499923);
#1202=CYLINDRICAL_SURFACE('',#13583,5.00000000000001);
#1203=CYLINDRICAL_SURFACE('',#13585,5.00000000000001);
#1204=CYLINDRICAL_SURFACE('',#13586,5.00000000000001);
#1205=CYLINDRICAL_SURFACE('',#13587,5.00000000000001);
#1206=CYLINDRICAL_SURFACE('',#13588,5.00000000000001);
#1207=CYLINDRICAL_SURFACE('',#13589,5.00000000000001);
#1208=CYLINDRICAL_SURFACE('',#13590,5.00000000000001);
#1209=CYLINDRICAL_SURFACE('',#13591,5.00000000000001);
#1210=CYLINDRICAL_SURFACE('',#13592,5.00000000000001);
#1211=CYLINDRICAL_SURFACE('',#13593,5.00000000000001);
#1212=CYLINDRICAL_SURFACE('',#13594,5.00000000000001);
#1213=CYLINDRICAL_SURFACE('',#13595,5.00000000000001);
#1214=CYLINDRICAL_SURFACE('',#13596,5.00000000000001);
#1215=CYLINDRICAL_SURFACE('',#13598,9.99999999999999);
#1216=CYLINDRICAL_SURFACE('',#13604,5.);
#1217=CYLINDRICAL_SURFACE('',#13607,5.);
#1218=CYLINDRICAL_SURFACE('',#13637,9.);
#1219=CYLINDRICAL_SURFACE('',#13638,9.);
#1220=CYLINDRICAL_SURFACE('',#13648,4.45873412499923);
#1221=CYLINDRICAL_SURFACE('',#13649,4.99999999999998);
#1222=CYLINDRICAL_SURFACE('',#13650,4.99999999999998);
#1223=CYLINDRICAL_SURFACE('',#13651,2.00000000000001);
#1224=CYLINDRICAL_SURFACE('',#13652,2.00000000000001);
#1225=CYLINDRICAL_SURFACE('',#13653,5.54126587500002);
#1226=CYLINDRICAL_SURFACE('',#13655,5.54126587500002);
#1227=CYLINDRICAL_SURFACE('',#13656,5.54126587500002);
#1228=CYLINDRICAL_SURFACE('',#13657,5.54126587500002);
#1229=CYLINDRICAL_SURFACE('',#13658,5.54126587500002);
#1230=CYLINDRICAL_SURFACE('',#13659,5.54126587500002);
#1231=CYLINDRICAL_SURFACE('',#13660,5.54126587500002);
#1232=CYLINDRICAL_SURFACE('',#13661,5.54126587500002);
#1233=CYLINDRICAL_SURFACE('',#13662,5.);
#1234=CYLINDRICAL_SURFACE('',#13664,5.);
#1235=CYLINDRICAL_SURFACE('',#13665,5.);
#1236=CYLINDRICAL_SURFACE('',#13666,5.);
#1237=CYLINDRICAL_SURFACE('',#13667,5.);
#1238=CYLINDRICAL_SURFACE('',#13668,5.);
#1239=CYLINDRICAL_SURFACE('',#13669,5.);
#1240=CYLINDRICAL_SURFACE('',#13670,5.);
#1241=CYLINDRICAL_SURFACE('',#13672,5.);
#1242=CYLINDRICAL_SURFACE('',#13673,9.99999999999999);
#1243=CYLINDRICAL_SURFACE('',#13686,5.54126587500002);
#1244=CYLINDRICAL_SURFACE('',#13701,10.);
#1245=CYLINDRICAL_SURFACE('',#13703,6.);
#1246=CYLINDRICAL_SURFACE('',#13716,7.50000000000001);
#1247=FACE_OUTER_BOUND('',#1944,.T.);
#1248=FACE_OUTER_BOUND('',#1945,.T.);
#1249=FACE_OUTER_BOUND('',#1946,.T.);
#1250=FACE_OUTER_BOUND('',#1947,.T.);
#1251=FACE_OUTER_BOUND('',#1948,.T.);
#1252=FACE_OUTER_BOUND('',#1949,.T.);
#1253=FACE_OUTER_BOUND('',#1950,.T.);
#1254=FACE_OUTER_BOUND('',#1951,.T.);
#1255=FACE_OUTER_BOUND('',#1952,.T.);
#1256=FACE_OUTER_BOUND('',#1953,.T.);
#1257=FACE_OUTER_BOUND('',#1954,.T.);
#1258=FACE_OUTER_BOUND('',#1955,.T.);
#1259=FACE_OUTER_BOUND('',#1956,.T.);
#1260=FACE_OUTER_BOUND('',#1957,.T.);
#1261=FACE_OUTER_BOUND('',#1958,.T.);
#1262=FACE_OUTER_BOUND('',#1959,.T.);
#1263=FACE_OUTER_BOUND('',#1960,.T.);
#1264=FACE_OUTER_BOUND('',#1961,.T.);
#1265=FACE_OUTER_BOUND('',#1962,.T.);
#1266=FACE_OUTER_BOUND('',#1963,.T.);
#1267=FACE_OUTER_BOUND('',#1964,.T.);
#1268=FACE_OUTER_BOUND('',#1965,.T.);
#1269=FACE_OUTER_BOUND('',#1966,.T.);
#1270=FACE_OUTER_BOUND('',#1967,.T.);
#1271=FACE_OUTER_BOUND('',#1968,.T.);
#1272=FACE_OUTER_BOUND('',#1969,.T.);
#1273=FACE_OUTER_BOUND('',#1970,.T.);
#1274=FACE_OUTER_BOUND('',#1971,.T.);
#1275=FACE_OUTER_BOUND('',#1972,.T.);
#1276=FACE_OUTER_BOUND('',#1973,.T.);
#1277=FACE_OUTER_BOUND('',#1974,.T.);
#1278=FACE_OUTER_BOUND('',#1975,.T.);
#1279=FACE_OUTER_BOUND('',#1976,.T.);
#1280=FACE_OUTER_BOUND('',#1977,.T.);
#1281=FACE_OUTER_BOUND('',#1978,.T.);
#1282=FACE_OUTER_BOUND('',#1979,.T.);
#1283=FACE_OUTER_BOUND('',#1980,.T.);
#1284=FACE_OUTER_BOUND('',#1981,.T.);
#1285=FACE_OUTER_BOUND('',#1982,.T.);
#1286=FACE_OUTER_BOUND('',#1983,.T.);
#1287=FACE_OUTER_BOUND('',#1984,.T.);
#1288=FACE_OUTER_BOUND('',#1985,.T.);
#1289=FACE_OUTER_BOUND('',#1986,.T.);
#1290=FACE_OUTER_BOUND('',#1987,.T.);
#1291=FACE_OUTER_BOUND('',#1988,.T.);
#1292=FACE_OUTER_BOUND('',#1989,.T.);
#1293=FACE_OUTER_BOUND('',#1990,.T.);
#1294=FACE_OUTER_BOUND('',#1991,.T.);
#1295=FACE_OUTER_BOUND('',#1992,.T.);
#1296=FACE_OUTER_BOUND('',#1993,.T.);
#1297=FACE_OUTER_BOUND('',#1994,.T.);
#1298=FACE_OUTER_BOUND('',#1995,.T.);
#1299=FACE_OUTER_BOUND('',#1996,.T.);
#1300=FACE_OUTER_BOUND('',#1997,.T.);
#1301=FACE_OUTER_BOUND('',#1998,.T.);
#1302=FACE_OUTER_BOUND('',#1999,.T.);
#1303=FACE_OUTER_BOUND('',#2000,.T.);
#1304=FACE_OUTER_BOUND('',#2006,.T.);
#1305=FACE_OUTER_BOUND('',#2010,.T.);
#1306=FACE_OUTER_BOUND('',#2011,.T.);
#1307=FACE_OUTER_BOUND('',#2012,.T.);
#1308=FACE_OUTER_BOUND('',#2013,.T.);
#1309=FACE_OUTER_BOUND('',#2019,.T.);
#1310=FACE_OUTER_BOUND('',#2020,.T.);
#1311=FACE_OUTER_BOUND('',#2021,.T.);
#1312=FACE_OUTER_BOUND('',#2022,.T.);
#1313=FACE_OUTER_BOUND('',#2023,.T.);
#1314=FACE_OUTER_BOUND('',#2025,.T.);
#1315=FACE_OUTER_BOUND('',#2026,.T.);
#1316=FACE_OUTER_BOUND('',#2027,.T.);
#1317=FACE_OUTER_BOUND('',#2028,.T.);
#1318=FACE_OUTER_BOUND('',#2030,.T.);
#1319=FACE_OUTER_BOUND('',#2031,.T.);
#1320=FACE_OUTER_BOUND('',#2032,.T.);
#1321=FACE_OUTER_BOUND('',#2033,.T.);
#1322=FACE_OUTER_BOUND('',#2035,.T.);
#1323=FACE_OUTER_BOUND('',#2036,.T.);
#1324=FACE_OUTER_BOUND('',#2037,.T.);
#1325=FACE_OUTER_BOUND('',#2038,.T.);
#1326=FACE_OUTER_BOUND('',#2039,.T.);
#1327=FACE_OUTER_BOUND('',#2040,.T.);
#1328=FACE_OUTER_BOUND('',#2041,.T.);
#1329=FACE_OUTER_BOUND('',#2042,.T.);
#1330=FACE_OUTER_BOUND('',#2043,.T.);
#1331=FACE_OUTER_BOUND('',#2044,.T.);
#1332=FACE_OUTER_BOUND('',#2045,.T.);
#1333=FACE_OUTER_BOUND('',#2046,.T.);
#1334=FACE_OUTER_BOUND('',#2047,.T.);
#1335=FACE_OUTER_BOUND('',#2048,.T.);
#1336=FACE_OUTER_BOUND('',#2049,.T.);
#1337=FACE_OUTER_BOUND('',#2050,.T.);
#1338=FACE_OUTER_BOUND('',#2052,.T.);
#1339=FACE_OUTER_BOUND('',#2054,.T.);
#1340=FACE_OUTER_BOUND('',#2056,.T.);
#1341=FACE_OUTER_BOUND('',#2057,.T.);
#1342=FACE_OUTER_BOUND('',#2058,.T.);
#1343=FACE_OUTER_BOUND('',#2059,.T.);
#1344=FACE_OUTER_BOUND('',#2060,.T.);
#1345=FACE_OUTER_BOUND('',#2064,.T.);
#1346=FACE_OUTER_BOUND('',#2066,.T.);
#1347=FACE_OUTER_BOUND('',#2068,.T.);
#1348=FACE_OUTER_BOUND('',#2069,.T.);
#1349=FACE_OUTER_BOUND('',#2070,.T.);
#1350=FACE_OUTER_BOUND('',#2071,.T.);
#1351=FACE_OUTER_BOUND('',#2073,.T.);
#1352=FACE_OUTER_BOUND('',#2074,.T.);
#1353=FACE_OUTER_BOUND('',#2075,.T.);
#1354=FACE_OUTER_BOUND('',#2076,.T.);
#1355=FACE_OUTER_BOUND('',#2077,.T.);
#1356=FACE_OUTER_BOUND('',#2078,.T.);
#1357=FACE_OUTER_BOUND('',#2079,.T.);
#1358=FACE_OUTER_BOUND('',#2080,.T.);
#1359=FACE_OUTER_BOUND('',#2081,.T.);
#1360=FACE_OUTER_BOUND('',#2082,.T.);
#1361=FACE_OUTER_BOUND('',#2084,.T.);
#1362=FACE_OUTER_BOUND('',#2086,.T.);
#1363=FACE_OUTER_BOUND('',#2088,.T.);
#1364=FACE_OUTER_BOUND('',#2089,.T.);
#1365=FACE_OUTER_BOUND('',#2090,.T.);
#1366=FACE_OUTER_BOUND('',#2091,.T.);
#1367=FACE_OUTER_BOUND('',#2092,.T.);
#1368=FACE_OUTER_BOUND('',#2093,.T.);
#1369=FACE_OUTER_BOUND('',#2094,.T.);
#1370=FACE_OUTER_BOUND('',#2095,.T.);
#1371=FACE_OUTER_BOUND('',#2096,.T.);
#1372=FACE_OUTER_BOUND('',#2097,.T.);
#1373=FACE_OUTER_BOUND('',#2098,.T.);
#1374=FACE_OUTER_BOUND('',#2099,.T.);
#1375=FACE_OUTER_BOUND('',#2100,.T.);
#1376=FACE_OUTER_BOUND('',#2101,.T.);
#1377=FACE_OUTER_BOUND('',#2102,.T.);
#1378=FACE_OUTER_BOUND('',#2103,.T.);
#1379=FACE_OUTER_BOUND('',#2104,.T.);
#1380=FACE_OUTER_BOUND('',#2105,.T.);
#1381=FACE_OUTER_BOUND('',#2106,.T.);
#1382=FACE_OUTER_BOUND('',#2107,.T.);
#1383=FACE_OUTER_BOUND('',#2108,.T.);
#1384=FACE_OUTER_BOUND('',#2109,.T.);
#1385=FACE_OUTER_BOUND('',#2110,.T.);
#1386=FACE_OUTER_BOUND('',#2111,.T.);
#1387=FACE_OUTER_BOUND('',#2112,.T.);
#1388=FACE_OUTER_BOUND('',#2113,.T.);
#1389=FACE_OUTER_BOUND('',#2114,.T.);
#1390=FACE_OUTER_BOUND('',#2115,.T.);
#1391=FACE_OUTER_BOUND('',#2116,.T.);
#1392=FACE_OUTER_BOUND('',#2117,.T.);
#1393=FACE_OUTER_BOUND('',#2118,.T.);
#1394=FACE_OUTER_BOUND('',#2119,.T.);
#1395=FACE_OUTER_BOUND('',#2120,.T.);
#1396=FACE_OUTER_BOUND('',#2121,.T.);
#1397=FACE_OUTER_BOUND('',#2122,.T.);
#1398=FACE_OUTER_BOUND('',#2123,.T.);
#1399=FACE_OUTER_BOUND('',#2124,.T.);
#1400=FACE_OUTER_BOUND('',#2125,.T.);
#1401=FACE_OUTER_BOUND('',#2126,.T.);
#1402=FACE_OUTER_BOUND('',#2127,.T.);
#1403=FACE_OUTER_BOUND('',#2128,.T.);
#1404=FACE_OUTER_BOUND('',#2129,.T.);
#1405=FACE_OUTER_BOUND('',#2130,.T.);
#1406=FACE_OUTER_BOUND('',#2131,.T.);
#1407=FACE_OUTER_BOUND('',#2132,.T.);
#1408=FACE_OUTER_BOUND('',#2133,.T.);
#1409=FACE_OUTER_BOUND('',#2134,.T.);
#1410=FACE_OUTER_BOUND('',#2135,.T.);
#1411=FACE_OUTER_BOUND('',#2136,.T.);
#1412=FACE_OUTER_BOUND('',#2139,.T.);
#1413=FACE_OUTER_BOUND('',#2140,.T.);
#1414=FACE_OUTER_BOUND('',#2141,.T.);
#1415=FACE_OUTER_BOUND('',#2145,.T.);
#1416=FACE_OUTER_BOUND('',#2146,.T.);
#1417=FACE_OUTER_BOUND('',#2147,.T.);
#1418=FACE_OUTER_BOUND('',#2148,.T.);
#1419=FACE_OUTER_BOUND('',#2149,.T.);
#1420=FACE_OUTER_BOUND('',#2150,.T.);
#1421=FACE_OUTER_BOUND('',#2151,.T.);
#1422=FACE_OUTER_BOUND('',#2154,.T.);
#1423=FACE_OUTER_BOUND('',#2155,.T.);
#1424=FACE_OUTER_BOUND('',#2156,.T.);
#1425=FACE_OUTER_BOUND('',#2157,.T.);
#1426=FACE_OUTER_BOUND('',#2158,.T.);
#1427=FACE_OUTER_BOUND('',#2159,.T.);
#1428=FACE_OUTER_BOUND('',#2160,.T.);
#1429=FACE_OUTER_BOUND('',#2161,.T.);
#1430=FACE_OUTER_BOUND('',#2162,.T.);
#1431=FACE_OUTER_BOUND('',#2163,.T.);
#1432=FACE_OUTER_BOUND('',#2164,.T.);
#1433=FACE_OUTER_BOUND('',#2165,.T.);
#1434=FACE_OUTER_BOUND('',#2166,.T.);
#1435=FACE_OUTER_BOUND('',#2167,.T.);
#1436=FACE_OUTER_BOUND('',#2168,.T.);
#1437=FACE_OUTER_BOUND('',#2169,.T.);
#1438=FACE_OUTER_BOUND('',#2170,.T.);
#1439=FACE_OUTER_BOUND('',#2171,.T.);
#1440=FACE_OUTER_BOUND('',#2172,.T.);
#1441=FACE_OUTER_BOUND('',#2173,.T.);
#1442=FACE_OUTER_BOUND('',#2174,.T.);
#1443=FACE_OUTER_BOUND('',#2175,.T.);
#1444=FACE_OUTER_BOUND('',#2176,.T.);
#1445=FACE_OUTER_BOUND('',#2177,.T.);
#1446=FACE_OUTER_BOUND('',#2181,.T.);
#1447=FACE_OUTER_BOUND('',#2183,.T.);
#1448=FACE_OUTER_BOUND('',#2185,.T.);
#1449=FACE_OUTER_BOUND('',#2186,.T.);
#1450=FACE_OUTER_BOUND('',#2187,.T.);
#1451=FACE_OUTER_BOUND('',#2188,.T.);
#1452=FACE_OUTER_BOUND('',#2189,.T.);
#1453=FACE_OUTER_BOUND('',#2190,.T.);
#1454=FACE_OUTER_BOUND('',#2191,.T.);
#1455=FACE_OUTER_BOUND('',#2192,.T.);
#1456=FACE_OUTER_BOUND('',#2193,.T.);
#1457=FACE_OUTER_BOUND('',#2194,.T.);
#1458=FACE_OUTER_BOUND('',#2195,.T.);
#1459=FACE_OUTER_BOUND('',#2196,.T.);
#1460=FACE_OUTER_BOUND('',#2197,.T.);
#1461=FACE_OUTER_BOUND('',#2198,.T.);
#1462=FACE_OUTER_BOUND('',#2199,.T.);
#1463=FACE_OUTER_BOUND('',#2201,.T.);
#1464=FACE_OUTER_BOUND('',#2202,.T.);
#1465=FACE_OUTER_BOUND('',#2203,.T.);
#1466=FACE_OUTER_BOUND('',#2204,.T.);
#1467=FACE_OUTER_BOUND('',#2205,.T.);
#1468=FACE_OUTER_BOUND('',#2206,.T.);
#1469=FACE_OUTER_BOUND('',#2207,.T.);
#1470=FACE_OUTER_BOUND('',#2208,.T.);
#1471=FACE_OUTER_BOUND('',#2210,.T.);
#1472=FACE_OUTER_BOUND('',#2211,.T.);
#1473=FACE_OUTER_BOUND('',#2212,.T.);
#1474=FACE_OUTER_BOUND('',#2213,.T.);
#1475=FACE_OUTER_BOUND('',#2214,.T.);
#1476=FACE_OUTER_BOUND('',#2216,.T.);
#1477=FACE_OUTER_BOUND('',#2217,.T.);
#1478=FACE_OUTER_BOUND('',#2218,.T.);
#1479=FACE_OUTER_BOUND('',#2219,.T.);
#1480=FACE_OUTER_BOUND('',#2220,.T.);
#1481=FACE_OUTER_BOUND('',#2221,.T.);
#1482=FACE_OUTER_BOUND('',#2222,.T.);
#1483=FACE_OUTER_BOUND('',#2223,.T.);
#1484=FACE_OUTER_BOUND('',#2224,.T.);
#1485=FACE_OUTER_BOUND('',#2225,.T.);
#1486=FACE_OUTER_BOUND('',#2226,.T.);
#1487=FACE_OUTER_BOUND('',#2227,.T.);
#1488=FACE_OUTER_BOUND('',#2228,.T.);
#1489=FACE_OUTER_BOUND('',#2229,.T.);
#1490=FACE_OUTER_BOUND('',#2230,.T.);
#1491=FACE_OUTER_BOUND('',#2231,.T.);
#1492=FACE_OUTER_BOUND('',#2232,.T.);
#1493=FACE_OUTER_BOUND('',#2233,.T.);
#1494=FACE_OUTER_BOUND('',#2234,.T.);
#1495=FACE_OUTER_BOUND('',#2235,.T.);
#1496=FACE_OUTER_BOUND('',#2236,.T.);
#1497=FACE_OUTER_BOUND('',#2237,.T.);
#1498=FACE_OUTER_BOUND('',#2238,.T.);
#1499=FACE_OUTER_BOUND('',#2239,.T.);
#1500=FACE_OUTER_BOUND('',#2240,.T.);
#1501=FACE_OUTER_BOUND('',#2241,.T.);
#1502=FACE_OUTER_BOUND('',#2242,.T.);
#1503=FACE_OUTER_BOUND('',#2243,.T.);
#1504=FACE_OUTER_BOUND('',#2244,.T.);
#1505=FACE_OUTER_BOUND('',#2245,.T.);
#1506=FACE_OUTER_BOUND('',#2246,.T.);
#1507=FACE_OUTER_BOUND('',#2247,.T.);
#1508=FACE_OUTER_BOUND('',#2248,.T.);
#1509=FACE_OUTER_BOUND('',#2249,.T.);
#1510=FACE_OUTER_BOUND('',#2250,.T.);
#1511=FACE_OUTER_BOUND('',#2251,.T.);
#1512=FACE_OUTER_BOUND('',#2252,.T.);
#1513=FACE_OUTER_BOUND('',#2253,.T.);
#1514=FACE_OUTER_BOUND('',#2254,.T.);
#1515=FACE_OUTER_BOUND('',#2255,.T.);
#1516=FACE_OUTER_BOUND('',#2256,.T.);
#1517=FACE_OUTER_BOUND('',#2257,.T.);
#1518=FACE_OUTER_BOUND('',#2258,.T.);
#1519=FACE_OUTER_BOUND('',#2259,.T.);
#1520=FACE_OUTER_BOUND('',#2262,.T.);
#1521=FACE_OUTER_BOUND('',#2265,.T.);
#1522=FACE_OUTER_BOUND('',#2267,.T.);
#1523=FACE_OUTER_BOUND('',#2269,.T.);
#1524=FACE_OUTER_BOUND('',#2270,.T.);
#1525=FACE_OUTER_BOUND('',#2271,.T.);
#1526=FACE_OUTER_BOUND('',#2273,.T.);
#1527=FACE_OUTER_BOUND('',#2274,.T.);
#1528=FACE_OUTER_BOUND('',#2275,.T.);
#1529=FACE_OUTER_BOUND('',#2277,.T.);
#1530=FACE_OUTER_BOUND('',#2280,.T.);
#1531=FACE_OUTER_BOUND('',#2283,.T.);
#1532=FACE_OUTER_BOUND('',#2285,.T.);
#1533=FACE_OUTER_BOUND('',#2286,.T.);
#1534=FACE_OUTER_BOUND('',#2287,.T.);
#1535=FACE_OUTER_BOUND('',#2288,.T.);
#1536=FACE_OUTER_BOUND('',#2290,.T.);
#1537=FACE_OUTER_BOUND('',#2292,.T.);
#1538=FACE_OUTER_BOUND('',#2293,.T.);
#1539=FACE_OUTER_BOUND('',#2294,.T.);
#1540=FACE_OUTER_BOUND('',#2295,.T.);
#1541=FACE_OUTER_BOUND('',#2296,.T.);
#1542=FACE_OUTER_BOUND('',#2297,.T.);
#1543=FACE_OUTER_BOUND('',#2298,.T.);
#1544=FACE_OUTER_BOUND('',#2299,.T.);
#1545=FACE_OUTER_BOUND('',#2300,.T.);
#1546=FACE_OUTER_BOUND('',#2301,.T.);
#1547=FACE_OUTER_BOUND('',#2302,.T.);
#1548=FACE_OUTER_BOUND('',#2303,.T.);
#1549=FACE_OUTER_BOUND('',#2304,.T.);
#1550=FACE_OUTER_BOUND('',#2305,.T.);
#1551=FACE_OUTER_BOUND('',#2306,.T.);
#1552=FACE_OUTER_BOUND('',#2307,.T.);
#1553=FACE_OUTER_BOUND('',#2308,.T.);
#1554=FACE_OUTER_BOUND('',#2311,.T.);
#1555=FACE_OUTER_BOUND('',#2314,.T.);
#1556=FACE_OUTER_BOUND('',#2315,.T.);
#1557=FACE_OUTER_BOUND('',#2316,.T.);
#1558=FACE_OUTER_BOUND('',#2317,.T.);
#1559=FACE_OUTER_BOUND('',#2318,.T.);
#1560=FACE_OUTER_BOUND('',#2319,.T.);
#1561=FACE_OUTER_BOUND('',#2320,.T.);
#1562=FACE_OUTER_BOUND('',#2321,.T.);
#1563=FACE_OUTER_BOUND('',#2322,.T.);
#1564=FACE_OUTER_BOUND('',#2323,.T.);
#1565=FACE_OUTER_BOUND('',#2324,.T.);
#1566=FACE_OUTER_BOUND('',#2325,.T.);
#1567=FACE_OUTER_BOUND('',#2326,.T.);
#1568=FACE_OUTER_BOUND('',#2328,.T.);
#1569=FACE_OUTER_BOUND('',#2329,.T.);
#1570=FACE_OUTER_BOUND('',#2330,.T.);
#1571=FACE_OUTER_BOUND('',#2331,.T.);
#1572=FACE_OUTER_BOUND('',#2332,.T.);
#1573=FACE_OUTER_BOUND('',#2333,.T.);
#1574=FACE_OUTER_BOUND('',#2334,.T.);
#1575=FACE_OUTER_BOUND('',#2335,.T.);
#1576=FACE_OUTER_BOUND('',#2336,.T.);
#1577=FACE_OUTER_BOUND('',#2337,.T.);
#1578=FACE_OUTER_BOUND('',#2338,.T.);
#1579=FACE_OUTER_BOUND('',#2339,.T.);
#1580=FACE_OUTER_BOUND('',#2340,.T.);
#1581=FACE_OUTER_BOUND('',#2342,.T.);
#1582=FACE_OUTER_BOUND('',#2343,.T.);
#1583=FACE_OUTER_BOUND('',#2344,.T.);
#1584=FACE_OUTER_BOUND('',#2346,.T.);
#1585=FACE_OUTER_BOUND('',#2348,.T.);
#1586=FACE_OUTER_BOUND('',#2349,.T.);
#1587=FACE_OUTER_BOUND('',#2350,.T.);
#1588=FACE_OUTER_BOUND('',#2352,.T.);
#1589=FACE_OUTER_BOUND('',#2354,.T.);
#1590=FACE_OUTER_BOUND('',#2356,.T.);
#1591=FACE_OUTER_BOUND('',#2358,.T.);
#1592=FACE_OUTER_BOUND('',#2359,.T.);
#1593=FACE_OUTER_BOUND('',#2360,.T.);
#1594=FACE_OUTER_BOUND('',#2361,.T.);
#1595=FACE_OUTER_BOUND('',#2362,.T.);
#1596=FACE_OUTER_BOUND('',#2363,.T.);
#1597=FACE_OUTER_BOUND('',#2364,.T.);
#1598=FACE_OUTER_BOUND('',#2366,.T.);
#1599=FACE_OUTER_BOUND('',#2367,.T.);
#1600=FACE_OUTER_BOUND('',#2368,.T.);
#1601=FACE_OUTER_BOUND('',#2370,.T.);
#1602=FACE_OUTER_BOUND('',#2372,.T.);
#1603=FACE_OUTER_BOUND('',#2373,.T.);
#1604=FACE_OUTER_BOUND('',#2374,.T.);
#1605=FACE_OUTER_BOUND('',#2375,.T.);
#1606=FACE_OUTER_BOUND('',#2376,.T.);
#1607=FACE_OUTER_BOUND('',#2377,.T.);
#1608=FACE_OUTER_BOUND('',#2378,.T.);
#1609=FACE_OUTER_BOUND('',#2379,.T.);
#1610=FACE_OUTER_BOUND('',#2380,.T.);
#1611=FACE_OUTER_BOUND('',#2381,.T.);
#1612=FACE_OUTER_BOUND('',#2382,.T.);
#1613=FACE_OUTER_BOUND('',#2383,.T.);
#1614=FACE_OUTER_BOUND('',#2384,.T.);
#1615=FACE_OUTER_BOUND('',#2385,.T.);
#1616=FACE_OUTER_BOUND('',#2386,.T.);
#1617=FACE_OUTER_BOUND('',#2387,.T.);
#1618=FACE_OUTER_BOUND('',#2388,.T.);
#1619=FACE_OUTER_BOUND('',#2389,.T.);
#1620=FACE_OUTER_BOUND('',#2391,.T.);
#1621=FACE_OUTER_BOUND('',#2392,.T.);
#1622=FACE_OUTER_BOUND('',#2393,.T.);
#1623=FACE_OUTER_BOUND('',#2394,.T.);
#1624=FACE_OUTER_BOUND('',#2395,.T.);
#1625=FACE_OUTER_BOUND('',#2396,.T.);
#1626=FACE_OUTER_BOUND('',#2397,.T.);
#1627=FACE_OUTER_BOUND('',#2398,.T.);
#1628=FACE_OUTER_BOUND('',#2399,.T.);
#1629=FACE_OUTER_BOUND('',#2400,.T.);
#1630=FACE_OUTER_BOUND('',#2401,.T.);
#1631=FACE_OUTER_BOUND('',#2402,.T.);
#1632=FACE_OUTER_BOUND('',#2403,.T.);
#1633=FACE_OUTER_BOUND('',#2404,.T.);
#1634=FACE_OUTER_BOUND('',#2406,.T.);
#1635=FACE_OUTER_BOUND('',#2407,.T.);
#1636=FACE_OUTER_BOUND('',#2408,.T.);
#1637=FACE_OUTER_BOUND('',#2409,.T.);
#1638=FACE_OUTER_BOUND('',#2410,.T.);
#1639=FACE_OUTER_BOUND('',#2411,.T.);
#1640=FACE_OUTER_BOUND('',#2412,.T.);
#1641=FACE_OUTER_BOUND('',#2413,.T.);
#1642=FACE_OUTER_BOUND('',#2414,.T.);
#1643=FACE_OUTER_BOUND('',#2415,.T.);
#1644=FACE_OUTER_BOUND('',#2416,.T.);
#1645=FACE_OUTER_BOUND('',#2417,.T.);
#1646=FACE_OUTER_BOUND('',#2418,.T.);
#1647=FACE_OUTER_BOUND('',#2419,.T.);
#1648=FACE_OUTER_BOUND('',#2420,.T.);
#1649=FACE_OUTER_BOUND('',#2421,.T.);
#1650=FACE_OUTER_BOUND('',#2422,.T.);
#1651=FACE_OUTER_BOUND('',#2423,.T.);
#1652=FACE_OUTER_BOUND('',#2424,.T.);
#1653=FACE_OUTER_BOUND('',#2425,.T.);
#1654=FACE_OUTER_BOUND('',#2426,.T.);
#1655=FACE_OUTER_BOUND('',#2427,.T.);
#1656=FACE_OUTER_BOUND('',#2428,.T.);
#1657=FACE_OUTER_BOUND('',#2429,.T.);
#1658=FACE_OUTER_BOUND('',#2430,.T.);
#1659=FACE_OUTER_BOUND('',#2431,.T.);
#1660=FACE_OUTER_BOUND('',#2432,.T.);
#1661=FACE_OUTER_BOUND('',#2433,.T.);
#1662=FACE_OUTER_BOUND('',#2434,.T.);
#1663=FACE_OUTER_BOUND('',#2435,.T.);
#1664=FACE_OUTER_BOUND('',#2436,.T.);
#1665=FACE_OUTER_BOUND('',#2437,.T.);
#1666=FACE_OUTER_BOUND('',#2438,.T.);
#1667=FACE_OUTER_BOUND('',#2439,.T.);
#1668=FACE_OUTER_BOUND('',#2440,.T.);
#1669=FACE_OUTER_BOUND('',#2441,.T.);
#1670=FACE_OUTER_BOUND('',#2442,.T.);
#1671=FACE_OUTER_BOUND('',#2444,.T.);
#1672=FACE_OUTER_BOUND('',#2446,.T.);
#1673=FACE_OUTER_BOUND('',#2448,.T.);
#1674=FACE_OUTER_BOUND('',#2450,.T.);
#1675=FACE_OUTER_BOUND('',#2451,.T.);
#1676=FACE_OUTER_BOUND('',#2452,.T.);
#1677=FACE_OUTER_BOUND('',#2453,.T.);
#1678=FACE_OUTER_BOUND('',#2454,.T.);
#1679=FACE_OUTER_BOUND('',#2455,.T.);
#1680=FACE_OUTER_BOUND('',#2456,.T.);
#1681=FACE_OUTER_BOUND('',#2457,.T.);
#1682=FACE_OUTER_BOUND('',#2458,.T.);
#1683=FACE_OUTER_BOUND('',#2459,.T.);
#1684=FACE_OUTER_BOUND('',#2460,.T.);
#1685=FACE_OUTER_BOUND('',#2461,.T.);
#1686=FACE_OUTER_BOUND('',#2462,.T.);
#1687=FACE_OUTER_BOUND('',#2463,.T.);
#1688=FACE_OUTER_BOUND('',#2464,.T.);
#1689=FACE_OUTER_BOUND('',#2465,.T.);
#1690=FACE_OUTER_BOUND('',#2466,.T.);
#1691=FACE_OUTER_BOUND('',#2467,.T.);
#1692=FACE_OUTER_BOUND('',#2468,.T.);
#1693=FACE_OUTER_BOUND('',#2469,.T.);
#1694=FACE_OUTER_BOUND('',#2470,.T.);
#1695=FACE_OUTER_BOUND('',#2471,.T.);
#1696=FACE_OUTER_BOUND('',#2472,.T.);
#1697=FACE_OUTER_BOUND('',#2473,.T.);
#1698=FACE_OUTER_BOUND('',#2474,.T.);
#1699=FACE_OUTER_BOUND('',#2475,.T.);
#1700=FACE_OUTER_BOUND('',#2476,.T.);
#1701=FACE_OUTER_BOUND('',#2477,.T.);
#1702=FACE_OUTER_BOUND('',#2478,.T.);
#1703=FACE_OUTER_BOUND('',#2479,.T.);
#1704=FACE_OUTER_BOUND('',#2480,.T.);
#1705=FACE_OUTER_BOUND('',#2481,.T.);
#1706=FACE_OUTER_BOUND('',#2482,.T.);
#1707=FACE_OUTER_BOUND('',#2483,.T.);
#1708=FACE_OUTER_BOUND('',#2484,.T.);
#1709=FACE_OUTER_BOUND('',#2485,.T.);
#1710=FACE_OUTER_BOUND('',#2486,.T.);
#1711=FACE_OUTER_BOUND('',#2487,.T.);
#1712=FACE_OUTER_BOUND('',#2488,.T.);
#1713=FACE_OUTER_BOUND('',#2489,.T.);
#1714=FACE_OUTER_BOUND('',#2490,.T.);
#1715=FACE_OUTER_BOUND('',#2491,.T.);
#1716=FACE_OUTER_BOUND('',#2493,.T.);
#1717=FACE_OUTER_BOUND('',#2494,.T.);
#1718=FACE_OUTER_BOUND('',#2495,.T.);
#1719=FACE_OUTER_BOUND('',#2496,.T.);
#1720=FACE_OUTER_BOUND('',#2497,.T.);
#1721=FACE_OUTER_BOUND('',#2498,.T.);
#1722=FACE_OUTER_BOUND('',#2499,.T.);
#1723=FACE_OUTER_BOUND('',#2500,.T.);
#1724=FACE_OUTER_BOUND('',#2501,.T.);
#1725=FACE_OUTER_BOUND('',#2502,.T.);
#1726=FACE_OUTER_BOUND('',#2503,.T.);
#1727=FACE_OUTER_BOUND('',#2504,.T.);
#1728=FACE_OUTER_BOUND('',#2505,.T.);
#1729=FACE_OUTER_BOUND('',#2507,.T.);
#1730=FACE_OUTER_BOUND('',#2508,.T.);
#1731=FACE_OUTER_BOUND('',#2509,.T.);
#1732=FACE_OUTER_BOUND('',#2510,.T.);
#1733=FACE_OUTER_BOUND('',#2511,.T.);
#1734=FACE_OUTER_BOUND('',#2512,.T.);
#1735=FACE_OUTER_BOUND('',#2513,.T.);
#1736=FACE_OUTER_BOUND('',#2514,.T.);
#1737=FACE_OUTER_BOUND('',#2515,.T.);
#1738=FACE_OUTER_BOUND('',#2516,.T.);
#1739=FACE_OUTER_BOUND('',#2517,.T.);
#1740=FACE_OUTER_BOUND('',#2518,.T.);
#1741=FACE_OUTER_BOUND('',#2519,.T.);
#1742=FACE_OUTER_BOUND('',#2520,.T.);
#1743=FACE_OUTER_BOUND('',#2521,.T.);
#1744=FACE_OUTER_BOUND('',#2522,.T.);
#1745=FACE_OUTER_BOUND('',#2523,.T.);
#1746=FACE_OUTER_BOUND('',#2524,.T.);
#1747=FACE_OUTER_BOUND('',#2525,.T.);
#1748=FACE_OUTER_BOUND('',#2526,.T.);
#1749=FACE_OUTER_BOUND('',#2527,.T.);
#1750=FACE_OUTER_BOUND('',#2528,.T.);
#1751=FACE_OUTER_BOUND('',#2529,.T.);
#1752=FACE_OUTER_BOUND('',#2530,.T.);
#1753=FACE_OUTER_BOUND('',#2531,.T.);
#1754=FACE_OUTER_BOUND('',#2532,.T.);
#1755=FACE_OUTER_BOUND('',#2533,.T.);
#1756=FACE_OUTER_BOUND('',#2534,.T.);
#1757=FACE_OUTER_BOUND('',#2535,.T.);
#1758=FACE_OUTER_BOUND('',#2536,.T.);
#1759=FACE_OUTER_BOUND('',#2537,.T.);
#1760=FACE_OUTER_BOUND('',#2538,.T.);
#1761=FACE_OUTER_BOUND('',#2539,.T.);
#1762=FACE_OUTER_BOUND('',#2540,.T.);
#1763=FACE_OUTER_BOUND('',#2541,.T.);
#1764=FACE_OUTER_BOUND('',#2543,.T.);
#1765=FACE_OUTER_BOUND('',#2544,.T.);
#1766=FACE_OUTER_BOUND('',#2545,.T.);
#1767=FACE_OUTER_BOUND('',#2546,.T.);
#1768=FACE_OUTER_BOUND('',#2547,.T.);
#1769=FACE_OUTER_BOUND('',#2550,.T.);
#1770=FACE_OUTER_BOUND('',#2553,.T.);
#1771=FACE_OUTER_BOUND('',#2554,.T.);
#1772=FACE_OUTER_BOUND('',#2555,.T.);
#1773=FACE_OUTER_BOUND('',#2556,.T.);
#1774=FACE_OUTER_BOUND('',#2557,.T.);
#1775=FACE_OUTER_BOUND('',#2560,.T.);
#1776=FACE_OUTER_BOUND('',#2563,.T.);
#1777=FACE_OUTER_BOUND('',#2564,.T.);
#1778=FACE_OUTER_BOUND('',#2565,.T.);
#1779=FACE_OUTER_BOUND('',#2566,.T.);
#1780=FACE_OUTER_BOUND('',#2567,.T.);
#1781=FACE_OUTER_BOUND('',#2568,.T.);
#1782=FACE_OUTER_BOUND('',#2569,.T.);
#1783=FACE_OUTER_BOUND('',#2570,.T.);
#1784=FACE_OUTER_BOUND('',#2571,.T.);
#1785=FACE_OUTER_BOUND('',#2572,.T.);
#1786=FACE_OUTER_BOUND('',#2574,.T.);
#1787=FACE_OUTER_BOUND('',#2575,.T.);
#1788=FACE_OUTER_BOUND('',#2576,.T.);
#1789=FACE_OUTER_BOUND('',#2577,.T.);
#1790=FACE_OUTER_BOUND('',#2578,.T.);
#1791=FACE_OUTER_BOUND('',#2579,.T.);
#1792=FACE_OUTER_BOUND('',#2581,.T.);
#1793=FACE_OUTER_BOUND('',#2582,.T.);
#1794=FACE_OUTER_BOUND('',#2583,.T.);
#1795=FACE_OUTER_BOUND('',#2584,.T.);
#1796=FACE_OUTER_BOUND('',#2585,.T.);
#1797=FACE_OUTER_BOUND('',#2586,.T.);
#1798=FACE_OUTER_BOUND('',#2587,.T.);
#1799=FACE_OUTER_BOUND('',#2588,.T.);
#1800=FACE_OUTER_BOUND('',#2589,.T.);
#1801=FACE_OUTER_BOUND('',#2590,.T.);
#1802=FACE_OUTER_BOUND('',#2591,.T.);
#1803=FACE_OUTER_BOUND('',#2592,.T.);
#1804=FACE_OUTER_BOUND('',#2593,.T.);
#1805=FACE_OUTER_BOUND('',#2594,.T.);
#1806=FACE_OUTER_BOUND('',#2595,.T.);
#1807=FACE_OUTER_BOUND('',#2596,.T.);
#1808=FACE_OUTER_BOUND('',#2597,.T.);
#1809=FACE_OUTER_BOUND('',#2598,.T.);
#1810=FACE_OUTER_BOUND('',#2599,.T.);
#1811=FACE_OUTER_BOUND('',#2601,.T.);
#1812=FACE_OUTER_BOUND('',#2603,.T.);
#1813=FACE_OUTER_BOUND('',#2605,.T.);
#1814=FACE_OUTER_BOUND('',#2607,.T.);
#1815=FACE_OUTER_BOUND('',#2609,.T.);
#1816=FACE_OUTER_BOUND('',#2611,.T.);
#1817=FACE_OUTER_BOUND('',#2612,.T.);
#1818=FACE_OUTER_BOUND('',#2613,.T.);
#1819=FACE_OUTER_BOUND('',#2614,.T.);
#1820=FACE_OUTER_BOUND('',#2615,.T.);
#1821=FACE_OUTER_BOUND('',#2616,.T.);
#1822=FACE_OUTER_BOUND('',#2617,.T.);
#1823=FACE_OUTER_BOUND('',#2618,.T.);
#1824=FACE_OUTER_BOUND('',#2619,.T.);
#1825=FACE_OUTER_BOUND('',#2620,.T.);
#1826=FACE_OUTER_BOUND('',#2621,.T.);
#1827=FACE_OUTER_BOUND('',#2622,.T.);
#1828=FACE_OUTER_BOUND('',#2623,.T.);
#1829=FACE_OUTER_BOUND('',#2625,.T.);
#1830=FACE_OUTER_BOUND('',#2627,.T.);
#1831=FACE_OUTER_BOUND('',#2629,.T.);
#1832=FACE_OUTER_BOUND('',#2631,.T.);
#1833=FACE_OUTER_BOUND('',#2633,.T.);
#1834=FACE_OUTER_BOUND('',#2635,.T.);
#1835=FACE_OUTER_BOUND('',#2636,.T.);
#1836=FACE_OUTER_BOUND('',#2637,.T.);
#1837=FACE_OUTER_BOUND('',#2638,.T.);
#1838=FACE_OUTER_BOUND('',#2639,.T.);
#1839=FACE_OUTER_BOUND('',#2640,.T.);
#1840=FACE_OUTER_BOUND('',#2641,.T.);
#1841=FACE_OUTER_BOUND('',#2642,.T.);
#1842=FACE_OUTER_BOUND('',#2643,.T.);
#1843=FACE_OUTER_BOUND('',#2644,.T.);
#1844=FACE_OUTER_BOUND('',#2645,.T.);
#1845=FACE_OUTER_BOUND('',#2646,.T.);
#1846=FACE_OUTER_BOUND('',#2647,.T.);
#1847=FACE_OUTER_BOUND('',#2648,.T.);
#1848=FACE_OUTER_BOUND('',#2649,.T.);
#1849=FACE_OUTER_BOUND('',#2650,.T.);
#1850=FACE_OUTER_BOUND('',#2651,.T.);
#1851=FACE_OUTER_BOUND('',#2652,.T.);
#1852=FACE_OUTER_BOUND('',#2653,.T.);
#1853=FACE_OUTER_BOUND('',#2654,.T.);
#1854=FACE_OUTER_BOUND('',#2655,.T.);
#1855=FACE_OUTER_BOUND('',#2656,.T.);
#1856=FACE_OUTER_BOUND('',#2657,.T.);
#1857=FACE_OUTER_BOUND('',#2658,.T.);
#1858=FACE_OUTER_BOUND('',#2659,.T.);
#1859=FACE_OUTER_BOUND('',#2660,.T.);
#1860=FACE_OUTER_BOUND('',#2661,.T.);
#1861=FACE_OUTER_BOUND('',#2662,.T.);
#1862=FACE_OUTER_BOUND('',#2663,.T.);
#1863=FACE_OUTER_BOUND('',#2664,.T.);
#1864=FACE_OUTER_BOUND('',#2665,.T.);
#1865=FACE_OUTER_BOUND('',#2666,.T.);
#1866=FACE_OUTER_BOUND('',#2667,.T.);
#1867=FACE_OUTER_BOUND('',#2668,.T.);
#1868=FACE_OUTER_BOUND('',#2669,.T.);
#1869=FACE_OUTER_BOUND('',#2670,.T.);
#1870=FACE_OUTER_BOUND('',#2671,.T.);
#1871=FACE_OUTER_BOUND('',#2672,.T.);
#1872=FACE_OUTER_BOUND('',#2674,.T.);
#1873=FACE_OUTER_BOUND('',#2676,.T.);
#1874=FACE_OUTER_BOUND('',#2677,.T.);
#1875=FACE_OUTER_BOUND('',#2679,.T.);
#1876=FACE_OUTER_BOUND('',#2681,.T.);
#1877=FACE_OUTER_BOUND('',#2682,.T.);
#1878=FACE_OUTER_BOUND('',#2683,.T.);
#1879=FACE_OUTER_BOUND('',#2684,.T.);
#1880=FACE_OUTER_BOUND('',#2685,.T.);
#1881=FACE_OUTER_BOUND('',#2686,.T.);
#1882=FACE_OUTER_BOUND('',#2687,.T.);
#1883=FACE_OUTER_BOUND('',#2688,.T.);
#1884=FACE_OUTER_BOUND('',#2689,.T.);
#1885=FACE_OUTER_BOUND('',#2690,.T.);
#1886=FACE_OUTER_BOUND('',#2692,.T.);
#1887=FACE_OUTER_BOUND('',#2693,.T.);
#1888=FACE_OUTER_BOUND('',#2694,.T.);
#1889=FACE_OUTER_BOUND('',#2695,.T.);
#1890=FACE_OUTER_BOUND('',#2696,.T.);
#1891=FACE_OUTER_BOUND('',#2697,.T.);
#1892=FACE_OUTER_BOUND('',#2698,.T.);
#1893=FACE_OUTER_BOUND('',#2699,.T.);
#1894=FACE_OUTER_BOUND('',#2700,.T.);
#1895=FACE_OUTER_BOUND('',#2701,.T.);
#1896=FACE_OUTER_BOUND('',#2702,.T.);
#1897=FACE_OUTER_BOUND('',#2703,.T.);
#1898=FACE_OUTER_BOUND('',#2704,.T.);
#1899=FACE_OUTER_BOUND('',#2705,.T.);
#1900=FACE_OUTER_BOUND('',#2706,.T.);
#1901=FACE_OUTER_BOUND('',#2707,.T.);
#1902=FACE_OUTER_BOUND('',#2708,.T.);
#1903=FACE_OUTER_BOUND('',#2709,.T.);
#1904=FACE_OUTER_BOUND('',#2710,.T.);
#1905=FACE_OUTER_BOUND('',#2711,.T.);
#1906=FACE_OUTER_BOUND('',#2712,.T.);
#1907=FACE_OUTER_BOUND('',#2713,.T.);
#1908=FACE_OUTER_BOUND('',#2714,.T.);
#1909=FACE_OUTER_BOUND('',#2715,.T.);
#1910=FACE_OUTER_BOUND('',#2716,.T.);
#1911=FACE_OUTER_BOUND('',#2717,.T.);
#1912=FACE_OUTER_BOUND('',#2718,.T.);
#1913=FACE_OUTER_BOUND('',#2719,.T.);
#1914=FACE_OUTER_BOUND('',#2721,.T.);
#1915=FACE_OUTER_BOUND('',#2723,.T.);
#1916=FACE_OUTER_BOUND('',#2725,.T.);
#1917=FACE_OUTER_BOUND('',#2726,.T.);
#1918=FACE_OUTER_BOUND('',#2727,.T.);
#1919=FACE_OUTER_BOUND('',#2728,.T.);
#1920=FACE_OUTER_BOUND('',#2729,.T.);
#1921=FACE_OUTER_BOUND('',#2730,.T.);
#1922=FACE_OUTER_BOUND('',#2731,.T.);
#1923=FACE_OUTER_BOUND('',#2732,.T.);
#1924=FACE_OUTER_BOUND('',#2733,.T.);
#1925=FACE_OUTER_BOUND('',#2734,.T.);
#1926=FACE_OUTER_BOUND('',#2735,.T.);
#1927=FACE_OUTER_BOUND('',#2736,.T.);
#1928=FACE_OUTER_BOUND('',#2737,.T.);
#1929=FACE_OUTER_BOUND('',#2738,.T.);
#1930=FACE_OUTER_BOUND('',#2739,.T.);
#1931=FACE_OUTER_BOUND('',#2740,.T.);
#1932=FACE_OUTER_BOUND('',#2741,.T.);
#1933=FACE_OUTER_BOUND('',#2742,.T.);
#1934=FACE_OUTER_BOUND('',#2743,.T.);
#1935=FACE_OUTER_BOUND('',#2744,.T.);
#1936=FACE_OUTER_BOUND('',#2745,.T.);
#1937=FACE_OUTER_BOUND('',#2746,.T.);
#1938=FACE_OUTER_BOUND('',#2747,.T.);
#1939=FACE_OUTER_BOUND('',#2749,.T.);
#1940=FACE_OUTER_BOUND('',#2750,.T.);
#1941=FACE_OUTER_BOUND('',#2751,.T.);
#1942=FACE_OUTER_BOUND('',#2752,.T.);
#1943=FACE_OUTER_BOUND('',#2753,.T.);
#1944=EDGE_LOOP('',(#7851,#7852,#7853,#7854));
#1945=EDGE_LOOP('',(#7855,#7856,#7857,#7858));
#1946=EDGE_LOOP('',(#7859,#7860,#7861,#7862));
#1947=EDGE_LOOP('',(#7863,#7864,#7865,#7866));
#1948=EDGE_LOOP('',(#7867,#7868,#7869,#7870));
#1949=EDGE_LOOP('',(#7871,#7872,#7873,#7874));
#1950=EDGE_LOOP('',(#7875,#7876,#7877,#7878,#7879));
#1951=EDGE_LOOP('',(#7880,#7881,#7882,#7883));
#1952=EDGE_LOOP('',(#7884,#7885,#7886,#7887));
#1953=EDGE_LOOP('',(#7888,#7889,#7890,#7891));
#1954=EDGE_LOOP('',(#7892,#7893,#7894,#7895));
#1955=EDGE_LOOP('',(#7896,#7897,#7898,#7899));
#1956=EDGE_LOOP('',(#7900,#7901,#7902,#7903,#7904));
#1957=EDGE_LOOP('',(#7905,#7906,#7907,#7908,#7909));
#1958=EDGE_LOOP('',(#7910,#7911,#7912,#7913,#7914));
#1959=EDGE_LOOP('',(#7915,#7916,#7917,#7918));
#1960=EDGE_LOOP('',(#7919,#7920,#7921,#7922,#7923));
#1961=EDGE_LOOP('',(#7924,#7925,#7926,#7927,#7928));
#1962=EDGE_LOOP('',(#7929,#7930,#7931,#7932,#7933,#7934));
#1963=EDGE_LOOP('',(#7935,#7936,#7937,#7938));
#1964=EDGE_LOOP('',(#7939,#7940,#7941,#7942));
#1965=EDGE_LOOP('',(#7943,#7944,#7945,#7946));
#1966=EDGE_LOOP('',(#7947,#7948,#7949,#7950,#7951,#7952));
#1967=EDGE_LOOP('',(#7953,#7954,#7955,#7956));
#1968=EDGE_LOOP('',(#7957,#7958,#7959,#7960));
#1969=EDGE_LOOP('',(#7961,#7962,#7963,#7964,#7965));
#1970=EDGE_LOOP('',(#7966,#7967,#7968,#7969));
#1971=EDGE_LOOP('',(#7970,#7971,#7972,#7973));
#1972=EDGE_LOOP('',(#7974,#7975,#7976,#7977));
#1973=EDGE_LOOP('',(#7978,#7979,#7980,#7981));
#1974=EDGE_LOOP('',(#7982,#7983,#7984,#7985,#7986,#7987));
#1975=EDGE_LOOP('',(#7988,#7989,#7990,#7991));
#1976=EDGE_LOOP('',(#7992,#7993,#7994,#7995,#7996));
#1977=EDGE_LOOP('',(#7997,#7998,#7999,#8000));
#1978=EDGE_LOOP('',(#8001,#8002,#8003,#8004));
#1979=EDGE_LOOP('',(#8005,#8006,#8007,#8008));
#1980=EDGE_LOOP('',(#8009,#8010,#8011,#8012,#8013));
#1981=EDGE_LOOP('',(#8014,#8015,#8016,#8017));
#1982=EDGE_LOOP('',(#8018,#8019,#8020,#8021));
#1983=EDGE_LOOP('',(#8022,#8023,#8024,#8025));
#1984=EDGE_LOOP('',(#8026,#8027,#8028,#8029,#8030));
#1985=EDGE_LOOP('',(#8031,#8032,#8033,#8034));
#1986=EDGE_LOOP('',(#8035,#8036,#8037,#8038,#8039));
#1987=EDGE_LOOP('',(#8040,#8041,#8042,#8043,#8044));
#1988=EDGE_LOOP('',(#8045,#8046,#8047,#8048));
#1989=EDGE_LOOP('',(#8049,#8050,#8051,#8052,#8053));
#1990=EDGE_LOOP('',(#8054,#8055,#8056,#8057,#8058,#8059,#8060,#8061));
#1991=EDGE_LOOP('',(#8062,#8063,#8064,#8065,#8066,#8067));
#1992=EDGE_LOOP('',(#8068,#8069,#8070,#8071));
#1993=EDGE_LOOP('',(#8072,#8073,#8074,#8075,#8076,#8077,#8078,#8079));
#1994=EDGE_LOOP('',(#8080,#8081,#8082,#8083));
#1995=EDGE_LOOP('',(#8084,#8085,#8086,#8087));
#1996=EDGE_LOOP('',(#8088,#8089,#8090,#8091));
#1997=EDGE_LOOP('',(#8092,#8093,#8094,#8095));
#1998=EDGE_LOOP('',(#8096,#8097,#8098,#8099,#8100,#8101,#8102,#8103));
#1999=EDGE_LOOP('',(#8104,#8105,#8106,#8107,#8108,#8109,#8110,#8111));
#2000=EDGE_LOOP('',(#8112,#8113,#8114,#8115,#8116,#8117,#8118,#8119,#8120,
#8121,#8122,#8123,#8124,#8125,#8126,#8127,#8128));
#2001=EDGE_LOOP('',(#8129));
#2002=EDGE_LOOP('',(#8130));
#2003=EDGE_LOOP('',(#8131));
#2004=EDGE_LOOP('',(#8132));
#2005=EDGE_LOOP('',(#8133,#8134,#8135,#8136,#8137,#8138,#8139,#8140));
#2006=EDGE_LOOP('',(#8141,#8142,#8143,#8144,#8145,#8146,#8147,#8148,#8149,
#8150,#8151,#8152,#8153,#8154,#8155,#8156,#8157,#8158,#8159));
#2007=EDGE_LOOP('',(#8160));
#2008=EDGE_LOOP('',(#8161));
#2009=EDGE_LOOP('',(#8162));
#2010=EDGE_LOOP('',(#8163,#8164,#8165,#8166));
#2011=EDGE_LOOP('',(#8167,#8168,#8169,#8170));
#2012=EDGE_LOOP('',(#8171,#8172,#8173,#8174));
#2013=EDGE_LOOP('',(#8175,#8176,#8177,#8178,#8179,#8180,#8181,#8182,#8183,
#8184,#8185,#8186,#8187,#8188,#8189,#8190,#8191));
#2014=EDGE_LOOP('',(#8192));
#2015=EDGE_LOOP('',(#8193));
#2016=EDGE_LOOP('',(#8194));
#2017=EDGE_LOOP('',(#8195));
#2018=EDGE_LOOP('',(#8196,#8197,#8198,#8199,#8200,#8201,#8202,#8203));
#2019=EDGE_LOOP('',(#8204,#8205,#8206,#8207));
#2020=EDGE_LOOP('',(#8208,#8209,#8210,#8211));
#2021=EDGE_LOOP('',(#8212,#8213,#8214,#8215));
#2022=EDGE_LOOP('',(#8216,#8217,#8218,#8219));
#2023=EDGE_LOOP('',(#8220));
#2024=EDGE_LOOP('',(#8221));
#2025=EDGE_LOOP('',(#8222,#8223,#8224,#8225,#8226,#8227,#8228,#8229));
#2026=EDGE_LOOP('',(#8230,#8231,#8232,#8233));
#2027=EDGE_LOOP('',(#8234,#8235,#8236,#8237,#8238,#8239,#8240,#8241));
#2028=EDGE_LOOP('',(#8242,#8243,#8244,#8245));
#2029=EDGE_LOOP('',(#8246));
#2030=EDGE_LOOP('',(#8247,#8248,#8249,#8250));
#2031=EDGE_LOOP('',(#8251,#8252,#8253,#8254));
#2032=EDGE_LOOP('',(#8255,#8256,#8257,#8258,#8259,#8260,#8261,#8262));
#2033=EDGE_LOOP('',(#8263,#8264,#8265,#8266));
#2034=EDGE_LOOP('',(#8267));
#2035=EDGE_LOOP('',(#8268,#8269,#8270,#8271,#8272,#8273,#8274,#8275));
#2036=EDGE_LOOP('',(#8276,#8277,#8278,#8279));
#2037=EDGE_LOOP('',(#8280,#8281,#8282,#8283,#8284,#8285,#8286,#8287));
#2038=EDGE_LOOP('',(#8288,#8289,#8290,#8291));
#2039=EDGE_LOOP('',(#8292,#8293,#8294,#8295,#8296,#8297,#8298,#8299));
#2040=EDGE_LOOP('',(#8300,#8301,#8302,#8303));
#2041=EDGE_LOOP('',(#8304,#8305,#8306,#8307));
#2042=EDGE_LOOP('',(#8308,#8309,#8310,#8311));
#2043=EDGE_LOOP('',(#8312,#8313,#8314,#8315));
#2044=EDGE_LOOP('',(#8316,#8317,#8318,#8319));
#2045=EDGE_LOOP('',(#8320,#8321,#8322,#8323,#8324,#8325));
#2046=EDGE_LOOP('',(#8326,#8327,#8328,#8329,#8330));
#2047=EDGE_LOOP('',(#8331,#8332,#8333,#8334));
#2048=EDGE_LOOP('',(#8335,#8336,#8337,#8338,#8339,#8340,#8341));
#2049=EDGE_LOOP('',(#8342,#8343,#8344,#8345,#8346,#8347,#8348,#8349));
#2050=EDGE_LOOP('',(#8350));
#2051=EDGE_LOOP('',(#8351));
#2052=EDGE_LOOP('',(#8352));
#2053=EDGE_LOOP('',(#8353));
#2054=EDGE_LOOP('',(#8354));
#2055=EDGE_LOOP('',(#8355));
#2056=EDGE_LOOP('',(#8356,#8357,#8358,#8359));
#2057=EDGE_LOOP('',(#8360,#8361,#8362,#8363));
#2058=EDGE_LOOP('',(#8364,#8365,#8366,#8367));
#2059=EDGE_LOOP('',(#8368,#8369,#8370,#8371));
#2060=EDGE_LOOP('',(#8372,#8373,#8374,#8375,#8376,#8377,#8378,#8379,#8380,
#8381,#8382,#8383,#8384,#8385,#8386,#8387,#8388,#8389,#8390));
#2061=EDGE_LOOP('',(#8391));
#2062=EDGE_LOOP('',(#8392));
#2063=EDGE_LOOP('',(#8393));
#2064=EDGE_LOOP('',(#8394));
#2065=EDGE_LOOP('',(#8395));
#2066=EDGE_LOOP('',(#8396,#8397,#8398,#8399));
#2067=EDGE_LOOP('',(#8400));
#2068=EDGE_LOOP('',(#8401,#8402,#8403,#8404,#8405));
#2069=EDGE_LOOP('',(#8406,#8407,#8408,#8409,#8410,#8411,#8412,#8413));
#2070=EDGE_LOOP('',(#8414,#8415,#8416,#8417,#8418,#8419,#8420,#8421));
#2071=EDGE_LOOP('',(#8422,#8423,#8424,#8425,#8426));
#2072=EDGE_LOOP('',(#8427));
#2073=EDGE_LOOP('',(#8428,#8429,#8430,#8431));
#2074=EDGE_LOOP('',(#8432,#8433,#8434,#8435));
#2075=EDGE_LOOP('',(#8436,#8437,#8438,#8439));
#2076=EDGE_LOOP('',(#8440,#8441,#8442,#8443));
#2077=EDGE_LOOP('',(#8444,#8445,#8446,#8447));
#2078=EDGE_LOOP('',(#8448,#8449,#8450,#8451,#8452,#8453,#8454));
#2079=EDGE_LOOP('',(#8455,#8456,#8457,#8458));
#2080=EDGE_LOOP('',(#8459,#8460,#8461,#8462,#8463));
#2081=EDGE_LOOP('',(#8464,#8465,#8466,#8467,#8468,#8469,#8470,#8471));
#2082=EDGE_LOOP('',(#8472));
#2083=EDGE_LOOP('',(#8473));
#2084=EDGE_LOOP('',(#8474));
#2085=EDGE_LOOP('',(#8475));
#2086=EDGE_LOOP('',(#8476));
#2087=EDGE_LOOP('',(#8477));
#2088=EDGE_LOOP('',(#8478,#8479,#8480,#8481));
#2089=EDGE_LOOP('',(#8482,#8483,#8484,#8485));
#2090=EDGE_LOOP('',(#8486,#8487,#8488,#8489));
#2091=EDGE_LOOP('',(#8490,#8491,#8492,#8493));
#2092=EDGE_LOOP('',(#8494,#8495,#8496,#8497,#8498,#8499,#8500,#8501));
#2093=EDGE_LOOP('',(#8502,#8503,#8504,#8505,#8506,#8507,#8508,#8509));
#2094=EDGE_LOOP('',(#8510,#8511,#8512,#8513));
#2095=EDGE_LOOP('',(#8514,#8515,#8516,#8517));
#2096=EDGE_LOOP('',(#8518,#8519,#8520,#8521));
#2097=EDGE_LOOP('',(#8522,#8523,#8524,#8525));
#2098=EDGE_LOOP('',(#8526,#8527,#8528,#8529,#8530));
#2099=EDGE_LOOP('',(#8531,#8532,#8533,#8534,#8535));
#2100=EDGE_LOOP('',(#8536,#8537,#8538,#8539));
#2101=EDGE_LOOP('',(#8540,#8541,#8542,#8543,#8544));
#2102=EDGE_LOOP('',(#8545,#8546,#8547,#8548,#8549));
#2103=EDGE_LOOP('',(#8550,#8551,#8552,#8553));
#2104=EDGE_LOOP('',(#8554,#8555,#8556));
#2105=EDGE_LOOP('',(#8557,#8558,#8559));
#2106=EDGE_LOOP('',(#8560,#8561,#8562,#8563));
#2107=EDGE_LOOP('',(#8564,#8565,#8566,#8567));
#2108=EDGE_LOOP('',(#8568,#8569,#8570,#8571));
#2109=EDGE_LOOP('',(#8572,#8573,#8574,#8575,#8576));
#2110=EDGE_LOOP('',(#8577,#8578,#8579,#8580,#8581));
#2111=EDGE_LOOP('',(#8582,#8583,#8584,#8585,#8586,#8587));
#2112=EDGE_LOOP('',(#8588,#8589,#8590,#8591,#8592,#8593));
#2113=EDGE_LOOP('',(#8594,#8595,#8596,#8597));
#2114=EDGE_LOOP('',(#8598,#8599,#8600,#8601));
#2115=EDGE_LOOP('',(#8602,#8603,#8604,#8605,#8606));
#2116=EDGE_LOOP('',(#8607,#8608,#8609,#8610,#8611));
#2117=EDGE_LOOP('',(#8612,#8613,#8614,#8615));
#2118=EDGE_LOOP('',(#8616,#8617,#8618,#8619));
#2119=EDGE_LOOP('',(#8620,#8621,#8622,#8623));
#2120=EDGE_LOOP('',(#8624,#8625,#8626,#8627));
#2121=EDGE_LOOP('',(#8628,#8629,#8630,#8631));
#2122=EDGE_LOOP('',(#8632,#8633,#8634,#8635));
#2123=EDGE_LOOP('',(#8636,#8637,#8638,#8639));
#2124=EDGE_LOOP('',(#8640,#8641,#8642,#8643));
#2125=EDGE_LOOP('',(#8644,#8645,#8646,#8647));
#2126=EDGE_LOOP('',(#8648,#8649,#8650,#8651,#8652,#8653));
#2127=EDGE_LOOP('',(#8654,#8655,#8656,#8657,#8658,#8659));
#2128=EDGE_LOOP('',(#8660,#8661,#8662,#8663,#8664,#8665));
#2129=EDGE_LOOP('',(#8666,#8667,#8668,#8669,#8670,#8671));
#2130=EDGE_LOOP('',(#8672,#8673,#8674,#8675,#8676));
#2131=EDGE_LOOP('',(#8677,#8678,#8679,#8680,#8681));
#2132=EDGE_LOOP('',(#8682,#8683,#8684,#8685,#8686));
#2133=EDGE_LOOP('',(#8687,#8688,#8689,#8690,#8691,#8692));
#2134=EDGE_LOOP('',(#8693,#8694,#8695,#8696,#8697,#8698));
#2135=EDGE_LOOP('',(#8699,#8700,#8701,#8702));
#2136=EDGE_LOOP('',(#8703,#8704,#8705,#8706,#8707,#8708,#8709,#8710,#8711,
#8712,#8713,#8714,#8715));
#2137=EDGE_LOOP('',(#8716));
#2138=EDGE_LOOP('',(#8717));
#2139=EDGE_LOOP('',(#8718,#8719,#8720,#8721));
#2140=EDGE_LOOP('',(#8722,#8723,#8724,#8725));
#2141=EDGE_LOOP('',(#8726,#8727,#8728,#8729,#8730,#8731,#8732,#8733,#8734,
#8735,#8736,#8737,#8738,#8739,#8740));
#2142=EDGE_LOOP('',(#8741));
#2143=EDGE_LOOP('',(#8742));
#2144=EDGE_LOOP('',(#8743));
#2145=EDGE_LOOP('',(#8744,#8745,#8746,#8747));
#2146=EDGE_LOOP('',(#8748,#8749,#8750,#8751));
#2147=EDGE_LOOP('',(#8752,#8753,#8754,#8755));
#2148=EDGE_LOOP('',(#8756,#8757,#8758,#8759));
#2149=EDGE_LOOP('',(#8760,#8761,#8762,#8763));
#2150=EDGE_LOOP('',(#8764,#8765,#8766,#8767,#8768));
#2151=EDGE_LOOP('',(#8769,#8770,#8771,#8772,#8773,#8774,#8775,#8776,#8777,
#8778,#8779,#8780,#8781));
#2152=EDGE_LOOP('',(#8782));
#2153=EDGE_LOOP('',(#8783));
#2154=EDGE_LOOP('',(#8784,#8785,#8786,#8787,#8788));
#2155=EDGE_LOOP('',(#8789,#8790,#8791,#8792));
#2156=EDGE_LOOP('',(#8793,#8794,#8795,#8796,#8797));
#2157=EDGE_LOOP('',(#8798,#8799,#8800,#8801,#8802));
#2158=EDGE_LOOP('',(#8803,#8804,#8805,#8806,#8807));
#2159=EDGE_LOOP('',(#8808,#8809,#8810,#8811));
#2160=EDGE_LOOP('',(#8812,#8813,#8814,#8815));
#2161=EDGE_LOOP('',(#8816,#8817,#8818,#8819));
#2162=EDGE_LOOP('',(#8820,#8821,#8822,#8823,#8824,#8825,#8826,#8827,#8828));
#2163=EDGE_LOOP('',(#8829,#8830,#8831,#8832));
#2164=EDGE_LOOP('',(#8833,#8834,#8835,#8836));
#2165=EDGE_LOOP('',(#8837,#8838,#8839,#8840));
#2166=EDGE_LOOP('',(#8841,#8842,#8843,#8844,#8845,#8846,#8847,#8848));
#2167=EDGE_LOOP('',(#8849,#8850,#8851,#8852));
#2168=EDGE_LOOP('',(#8853,#8854,#8855,#8856,#8857,#8858,#8859,#8860,#8861,
#8862));
#2169=EDGE_LOOP('',(#8863,#8864,#8865,#8866,#8867,#8868,#8869,#8870,#8871,
#8872));
#2170=EDGE_LOOP('',(#8873,#8874,#8875,#8876));
#2171=EDGE_LOOP('',(#8877,#8878,#8879,#8880));
#2172=EDGE_LOOP('',(#8881,#8882,#8883,#8884,#8885));
#2173=EDGE_LOOP('',(#8886,#8887,#8888,#8889));
#2174=EDGE_LOOP('',(#8890,#8891,#8892,#8893));
#2175=EDGE_LOOP('',(#8894,#8895,#8896,#8897));
#2176=EDGE_LOOP('',(#8898,#8899,#8900,#8901,#8902));
#2177=EDGE_LOOP('',(#8903,#8904,#8905,#8906,#8907,#8908,#8909,#8910,#8911,
#8912,#8913,#8914,#8915,#8916,#8917));
#2178=EDGE_LOOP('',(#8918));
#2179=EDGE_LOOP('',(#8919));
#2180=EDGE_LOOP('',(#8920));
#2181=EDGE_LOOP('',(#8921));
#2182=EDGE_LOOP('',(#8922));
#2183=EDGE_LOOP('',(#8923));
#2184=EDGE_LOOP('',(#8924));
#2185=EDGE_LOOP('',(#8925,#8926,#8927,#8928));
#2186=EDGE_LOOP('',(#8929,#8930,#8931,#8932));
#2187=EDGE_LOOP('',(#8933,#8934,#8935,#8936,#8937,#8938));
#2188=EDGE_LOOP('',(#8939,#8940,#8941,#8942,#8943,#8944));
#2189=EDGE_LOOP('',(#8945,#8946,#8947,#8948));
#2190=EDGE_LOOP('',(#8949,#8950,#8951,#8952));
#2191=EDGE_LOOP('',(#8953,#8954,#8955,#8956));
#2192=EDGE_LOOP('',(#8957,#8958,#8959,#8960));
#2193=EDGE_LOOP('',(#8961,#8962,#8963,#8964));
#2194=EDGE_LOOP('',(#8965,#8966,#8967,#8968));
#2195=EDGE_LOOP('',(#8969,#8970,#8971,#8972,#8973));
#2196=EDGE_LOOP('',(#8974,#8975,#8976,#8977));
#2197=EDGE_LOOP('',(#8978,#8979,#8980,#8981,#8982));
#2198=EDGE_LOOP('',(#8983));
#2199=EDGE_LOOP('',(#8984));
#2200=EDGE_LOOP('',(#8985));
#2201=EDGE_LOOP('',(#8986));
#2202=EDGE_LOOP('',(#8987,#8988,#8989,#8990));
#2203=EDGE_LOOP('',(#8991,#8992,#8993,#8994));
#2204=EDGE_LOOP('',(#8995,#8996,#8997,#8998,#8999));
#2205=EDGE_LOOP('',(#9000,#9001,#9002,#9003));
#2206=EDGE_LOOP('',(#9004,#9005,#9006,#9007,#9008));
#2207=EDGE_LOOP('',(#9009));
#2208=EDGE_LOOP('',(#9010));
#2209=EDGE_LOOP('',(#9011));
#2210=EDGE_LOOP('',(#9012));
#2211=EDGE_LOOP('',(#9013,#9014,#9015,#9016,#9017));
#2212=EDGE_LOOP('',(#9018,#9019,#9020,#9021));
#2213=EDGE_LOOP('',(#9022,#9023,#9024,#9025,#9026,#9027,#9028,#9029,#9030,
#9031,#9032,#9033,#9034,#9035,#9036,#9037));
#2214=EDGE_LOOP('',(#9038,#9039,#9040,#9041,#9042,#9043,#9044,#9045,#9046,
#9047,#9048,#9049,#9050,#9051,#9052,#9053));
#2215=EDGE_LOOP('',(#9054));
#2216=EDGE_LOOP('',(#9055,#9056,#9057,#9058,#9059));
#2217=EDGE_LOOP('',(#9060,#9061,#9062,#9063));
#2218=EDGE_LOOP('',(#9064,#9065,#9066,#9067));
#2219=EDGE_LOOP('',(#9068,#9069,#9070,#9071));
#2220=EDGE_LOOP('',(#9072));
#2221=EDGE_LOOP('',(#9073,#9074,#9075,#9076));
#2222=EDGE_LOOP('',(#9077,#9078,#9079,#9080));
#2223=EDGE_LOOP('',(#9081,#9082,#9083,#9084,#9085,#9086));
#2224=EDGE_LOOP('',(#9087,#9088,#9089,#9090,#9091,#9092));
#2225=EDGE_LOOP('',(#9093,#9094,#9095,#9096,#9097,#9098));
#2226=EDGE_LOOP('',(#9099,#9100,#9101,#9102,#9103,#9104));
#2227=EDGE_LOOP('',(#9105,#9106,#9107,#9108));
#2228=EDGE_LOOP('',(#9109,#9110,#9111,#9112));
#2229=EDGE_LOOP('',(#9113,#9114,#9115,#9116,#9117,#9118));
#2230=EDGE_LOOP('',(#9119,#9120,#9121,#9122,#9123,#9124));
#2231=EDGE_LOOP('',(#9125,#9126,#9127,#9128,#9129,#9130));
#2232=EDGE_LOOP('',(#9131,#9132,#9133,#9134,#9135,#9136));
#2233=EDGE_LOOP('',(#9137,#9138,#9139,#9140));
#2234=EDGE_LOOP('',(#9141,#9142,#9143,#9144));
#2235=EDGE_LOOP('',(#9145,#9146,#9147,#9148));
#2236=EDGE_LOOP('',(#9149,#9150,#9151,#9152));
#2237=EDGE_LOOP('',(#9153,#9154,#9155,#9156));
#2238=EDGE_LOOP('',(#9157,#9158,#9159,#9160));
#2239=EDGE_LOOP('',(#9161,#9162,#9163,#9164));
#2240=EDGE_LOOP('',(#9165,#9166,#9167,#9168));
#2241=EDGE_LOOP('',(#9169,#9170,#9171,#9172));
#2242=EDGE_LOOP('',(#9173,#9174,#9175,#9176,#9177));
#2243=EDGE_LOOP('',(#9178,#9179,#9180,#9181,#9182));
#2244=EDGE_LOOP('',(#9183,#9184,#9185,#9186,#9187,#9188));
#2245=EDGE_LOOP('',(#9189,#9190,#9191,#9192));
#2246=EDGE_LOOP('',(#9193,#9194,#9195,#9196,#9197,#9198,#9199,#9200));
#2247=EDGE_LOOP('',(#9201,#9202,#9203,#9204));
#2248=EDGE_LOOP('',(#9205,#9206,#9207,#9208));
#2249=EDGE_LOOP('',(#9209,#9210,#9211,#9212));
#2250=EDGE_LOOP('',(#9213,#9214,#9215,#9216));
#2251=EDGE_LOOP('',(#9217,#9218,#9219,#9220));
#2252=EDGE_LOOP('',(#9221,#9222,#9223,#9224));
#2253=EDGE_LOOP('',(#9225,#9226,#9227,#9228));
#2254=EDGE_LOOP('',(#9229,#9230,#9231,#9232,#9233,#9234));
#2255=EDGE_LOOP('',(#9235,#9236,#9237,#9238));
#2256=EDGE_LOOP('',(#9239,#9240,#9241,#9242,#9243,#9244,#9245));
#2257=EDGE_LOOP('',(#9246,#9247,#9248,#9249));
#2258=EDGE_LOOP('',(#9250,#9251,#9252,#9253));
#2259=EDGE_LOOP('',(#9254,#9255,#9256,#9257,#9258,#9259,#9260,#9261));
#2260=EDGE_LOOP('',(#9262));
#2261=EDGE_LOOP('',(#9263));
#2262=EDGE_LOOP('',(#9264,#9265,#9266,#9267,#9268,#9269,#9270,#9271));
#2263=EDGE_LOOP('',(#9272));
#2264=EDGE_LOOP('',(#9273));
#2265=EDGE_LOOP('',(#9274,#9275,#9276,#9277));
#2266=EDGE_LOOP('',(#9278));
#2267=EDGE_LOOP('',(#9279,#9280,#9281,#9282,#9283,#9284,#9285,#9286,#9287,
#9288));
#2268=EDGE_LOOP('',(#9289,#9290,#9291,#9292,#9293,#9294));
#2269=EDGE_LOOP('',(#9295,#9296,#9297,#9298));
#2270=EDGE_LOOP('',(#9299,#9300,#9301,#9302));
#2271=EDGE_LOOP('',(#9303,#9304,#9305,#9306,#9307,#9308,#9309,#9310,#9311,
#9312));
#2272=EDGE_LOOP('',(#9313,#9314,#9315,#9316,#9317,#9318));
#2273=EDGE_LOOP('',(#9319,#9320,#9321,#9322));
#2274=EDGE_LOOP('',(#9323,#9324,#9325,#9326));
#2275=EDGE_LOOP('',(#9327,#9328,#9329,#9330));
#2276=EDGE_LOOP('',(#9331));
#2277=EDGE_LOOP('',(#9332,#9333,#9334,#9335,#9336,#9337,#9338,#9339));
#2278=EDGE_LOOP('',(#9340));
#2279=EDGE_LOOP('',(#9341));
#2280=EDGE_LOOP('',(#9342,#9343,#9344,#9345,#9346,#9347,#9348,#9349));
#2281=EDGE_LOOP('',(#9350));
#2282=EDGE_LOOP('',(#9351));
#2283=EDGE_LOOP('',(#9352,#9353,#9354,#9355));
#2284=EDGE_LOOP('',(#9356));
#2285=EDGE_LOOP('',(#9357,#9358,#9359,#9360));
#2286=EDGE_LOOP('',(#9361,#9362,#9363,#9364));
#2287=EDGE_LOOP('',(#9365,#9366,#9367,#9368));
#2288=EDGE_LOOP('',(#9369));
#2289=EDGE_LOOP('',(#9370));
#2290=EDGE_LOOP('',(#9371));
#2291=EDGE_LOOP('',(#9372));
#2292=EDGE_LOOP('',(#9373,#9374,#9375,#9376));
#2293=EDGE_LOOP('',(#9377,#9378,#9379,#9380));
#2294=EDGE_LOOP('',(#9381,#9382,#9383,#9384));
#2295=EDGE_LOOP('',(#9385,#9386,#9387,#9388));
#2296=EDGE_LOOP('',(#9389,#9390,#9391,#9392));
#2297=EDGE_LOOP('',(#9393,#9394,#9395,#9396,#9397));
#2298=EDGE_LOOP('',(#9398,#9399,#9400,#9401,#9402));
#2299=EDGE_LOOP('',(#9403));
#2300=EDGE_LOOP('',(#9404));
#2301=EDGE_LOOP('',(#9405,#9406,#9407,#9408));
#2302=EDGE_LOOP('',(#9409,#9410,#9411,#9412,#9413));
#2303=EDGE_LOOP('',(#9414,#9415,#9416,#9417,#9418));
#2304=EDGE_LOOP('',(#9419));
#2305=EDGE_LOOP('',(#9420));
#2306=EDGE_LOOP('',(#9421,#9422,#9423,#9424));
#2307=EDGE_LOOP('',(#9425,#9426,#9427,#9428));
#2308=EDGE_LOOP('',(#9429,#9430,#9431,#9432,#9433,#9434,#9435,#9436));
#2309=EDGE_LOOP('',(#9437));
#2310=EDGE_LOOP('',(#9438));
#2311=EDGE_LOOP('',(#9439,#9440,#9441,#9442,#9443,#9444,#9445,#9446));
#2312=EDGE_LOOP('',(#9447));
#2313=EDGE_LOOP('',(#9448));
#2314=EDGE_LOOP('',(#9449,#9450,#9451,#9452));
#2315=EDGE_LOOP('',(#9453,#9454,#9455,#9456));
#2316=EDGE_LOOP('',(#9457,#9458,#9459,#9460));
#2317=EDGE_LOOP('',(#9461,#9462,#9463,#9464));
#2318=EDGE_LOOP('',(#9465,#9466,#9467,#9468));
#2319=EDGE_LOOP('',(#9469,#9470,#9471,#9472));
#2320=EDGE_LOOP('',(#9473,#9474,#9475,#9476));
#2321=EDGE_LOOP('',(#9477,#9478,#9479,#9480));
#2322=EDGE_LOOP('',(#9481,#9482,#9483,#9484,#9485));
#2323=EDGE_LOOP('',(#9486,#9487,#9488,#9489,#9490));
#2324=EDGE_LOOP('',(#9491,#9492,#9493,#9494,#9495));
#2325=EDGE_LOOP('',(#9496,#9497,#9498,#9499));
#2326=EDGE_LOOP('',(#9500,#9501,#9502,#9503));
#2327=EDGE_LOOP('',(#9504,#9505));
#2328=EDGE_LOOP('',(#9506,#9507,#9508,#9509));
#2329=EDGE_LOOP('',(#9510,#9511,#9512,#9513));
#2330=EDGE_LOOP('',(#9514,#9515,#9516,#9517,#9518,#9519,#9520));
#2331=EDGE_LOOP('',(#9521,#9522,#9523,#9524,#9525,#9526,#9527));
#2332=EDGE_LOOP('',(#9528,#9529,#9530,#9531,#9532,#9533,#9534,#9535,#9536));
#2333=EDGE_LOOP('',(#9537,#9538,#9539,#9540));
#2334=EDGE_LOOP('',(#9541,#9542,#9543,#9544));
#2335=EDGE_LOOP('',(#9545,#9546,#9547,#9548));
#2336=EDGE_LOOP('',(#9549,#9550,#9551,#9552));
#2337=EDGE_LOOP('',(#9553,#9554,#9555,#9556,#9557,#9558));
#2338=EDGE_LOOP('',(#9559,#9560,#9561,#9562,#9563,#9564,#9565,#9566,#9567,
#9568,#9569,#9570));
#2339=EDGE_LOOP('',(#9571,#9572,#9573,#9574,#9575,#9576,#9577,#9578,#9579,
#9580,#9581,#9582,#9583,#9584,#9585,#9586,#9587,#9588));
#2340=EDGE_LOOP('',(#9589,#9590,#9591,#9592));
#2341=EDGE_LOOP('',(#9593));
#2342=EDGE_LOOP('',(#9594,#9595,#9596,#9597));
#2343=EDGE_LOOP('',(#9598,#9599,#9600,#9601));
#2344=EDGE_LOOP('',(#9602));
#2345=EDGE_LOOP('',(#9603));
#2346=EDGE_LOOP('',(#9604));
#2347=EDGE_LOOP('',(#9605));
#2348=EDGE_LOOP('',(#9606,#9607,#9608,#9609,#9610));
#2349=EDGE_LOOP('',(#9611,#9612,#9613,#9614));
#2350=EDGE_LOOP('',(#9615));
#2351=EDGE_LOOP('',(#9616));
#2352=EDGE_LOOP('',(#9617));
#2353=EDGE_LOOP('',(#9618));
#2354=EDGE_LOOP('',(#9619));
#2355=EDGE_LOOP('',(#9620));
#2356=EDGE_LOOP('',(#9621));
#2357=EDGE_LOOP('',(#9622,#9623,#9624,#9625,#9626,#9627));
#2358=EDGE_LOOP('',(#9628,#9629,#9630,#9631));
#2359=EDGE_LOOP('',(#9632,#9633,#9634,#9635));
#2360=EDGE_LOOP('',(#9636,#9637,#9638,#9639));
#2361=EDGE_LOOP('',(#9640,#9641,#9642,#9643));
#2362=EDGE_LOOP('',(#9644,#9645,#9646,#9647));
#2363=EDGE_LOOP('',(#9648,#9649,#9650,#9651));
#2364=EDGE_LOOP('',(#9652,#9653,#9654,#9655,#9656,#9657));
#2365=EDGE_LOOP('',(#9658));
#2366=EDGE_LOOP('',(#9659,#9660,#9661,#9662,#9663,#9664,#9665,#9666));
#2367=EDGE_LOOP('',(#9667,#9668,#9669,#9670,#9671,#9672,#9673,#9674));
#2368=EDGE_LOOP('',(#9675,#9676,#9677,#9678,#9679));
#2369=EDGE_LOOP('',(#9680));
#2370=EDGE_LOOP('',(#9681,#9682,#9683,#9684,#9685));
#2371=EDGE_LOOP('',(#9686));
#2372=EDGE_LOOP('',(#9687,#9688,#9689,#9690));
#2373=EDGE_LOOP('',(#9691,#9692,#9693,#9694,#9695));
#2374=EDGE_LOOP('',(#9696,#9697,#9698,#9699));
#2375=EDGE_LOOP('',(#9700,#9701,#9702,#9703,#9704));
#2376=EDGE_LOOP('',(#9705,#9706,#9707,#9708));
#2377=EDGE_LOOP('',(#9709,#9710,#9711));
#2378=EDGE_LOOP('',(#9712,#9713,#9714));
#2379=EDGE_LOOP('',(#9715,#9716,#9717));
#2380=EDGE_LOOP('',(#9718,#9719,#9720));
#2381=EDGE_LOOP('',(#9721,#9722,#9723));
#2382=EDGE_LOOP('',(#9724,#9725,#9726));
#2383=EDGE_LOOP('',(#9727,#9728,#9729,#9730,#9731,#9732,#9733));
#2384=EDGE_LOOP('',(#9734,#9735,#9736,#9737,#9738,#9739,#9740));
#2385=EDGE_LOOP('',(#9741,#9742,#9743,#9744,#9745,#9746,#9747));
#2386=EDGE_LOOP('',(#9748,#9749,#9750,#9751,#9752,#9753,#9754));
#2387=EDGE_LOOP('',(#9755,#9756,#9757,#9758,#9759,#9760,#9761));
#2388=EDGE_LOOP('',(#9762,#9763,#9764,#9765,#9766,#9767,#9768));
#2389=EDGE_LOOP('',(#9769,#9770,#9771,#9772,#9773,#9774));
#2390=EDGE_LOOP('',(#9775));
#2391=EDGE_LOOP('',(#9776,#9777,#9778));
#2392=EDGE_LOOP('',(#9779,#9780,#9781));
#2393=EDGE_LOOP('',(#9782,#9783,#9784));
#2394=EDGE_LOOP('',(#9785,#9786,#9787));
#2395=EDGE_LOOP('',(#9788,#9789,#9790));
#2396=EDGE_LOOP('',(#9791,#9792,#9793));
#2397=EDGE_LOOP('',(#9794,#9795,#9796,#9797,#9798,#9799,#9800));
#2398=EDGE_LOOP('',(#9801,#9802,#9803,#9804,#9805,#9806,#9807));
#2399=EDGE_LOOP('',(#9808,#9809,#9810,#9811,#9812,#9813,#9814));
#2400=EDGE_LOOP('',(#9815,#9816,#9817,#9818,#9819,#9820,#9821));
#2401=EDGE_LOOP('',(#9822,#9823,#9824,#9825,#9826));
#2402=EDGE_LOOP('',(#9827,#9828,#9829,#9830,#9831));
#2403=EDGE_LOOP('',(#9832));
#2404=EDGE_LOOP('',(#9833));
#2405=EDGE_LOOP('',(#9834));
#2406=EDGE_LOOP('',(#9835,#9836,#9837,#9838));
#2407=EDGE_LOOP('',(#9839,#9840,#9841,#9842));
#2408=EDGE_LOOP('',(#9843,#9844,#9845));
#2409=EDGE_LOOP('',(#9846,#9847,#9848,#9849,#9850));
#2410=EDGE_LOOP('',(#9851,#9852,#9853,#9854));
#2411=EDGE_LOOP('',(#9855,#9856,#9857,#9858));
#2412=EDGE_LOOP('',(#9859,#9860,#9861,#9862));
#2413=EDGE_LOOP('',(#9863,#9864,#9865,#9866));
#2414=EDGE_LOOP('',(#9867,#9868,#9869,#9870));
#2415=EDGE_LOOP('',(#9871,#9872,#9873,#9874));
#2416=EDGE_LOOP('',(#9875,#9876,#9877,#9878));
#2417=EDGE_LOOP('',(#9879,#9880,#9881));
#2418=EDGE_LOOP('',(#9882,#9883,#9884,#9885,#9886));
#2419=EDGE_LOOP('',(#9887,#9888,#9889,#9890));
#2420=EDGE_LOOP('',(#9891,#9892,#9893,#9894));
#2421=EDGE_LOOP('',(#9895,#9896,#9897,#9898));
#2422=EDGE_LOOP('',(#9899,#9900,#9901,#9902));
#2423=EDGE_LOOP('',(#9903,#9904,#9905,#9906));
#2424=EDGE_LOOP('',(#9907,#9908,#9909,#9910));
#2425=EDGE_LOOP('',(#9911,#9912,#9913,#9914));
#2426=EDGE_LOOP('',(#9915,#9916,#9917,#9918,#9919,#9920,#9921,#9922));
#2427=EDGE_LOOP('',(#9923,#9924,#9925,#9926,#9927,#9928));
#2428=EDGE_LOOP('',(#9929,#9930,#9931,#9932,#9933,#9934));
#2429=EDGE_LOOP('',(#9935,#9936,#9937,#9938,#9939,#9940));
#2430=EDGE_LOOP('',(#9941,#9942,#9943,#9944,#9945));
#2431=EDGE_LOOP('',(#9946,#9947,#9948,#9949,#9950,#9951,#9952,#9953,#9954,
#9955,#9956));
#2432=EDGE_LOOP('',(#9957));
#2433=EDGE_LOOP('',(#9958));
#2434=EDGE_LOOP('',(#9959));
#2435=EDGE_LOOP('',(#9960));
#2436=EDGE_LOOP('',(#9961,#9962,#9963,#9964));
#2437=EDGE_LOOP('',(#9965,#9966,#9967,#9968));
#2438=EDGE_LOOP('',(#9969,#9970,#9971,#9972));
#2439=EDGE_LOOP('',(#9973,#9974,#9975,#9976));
#2440=EDGE_LOOP('',(#9977,#9978,#9979,#9980));
#2441=EDGE_LOOP('',(#9981));
#2442=EDGE_LOOP('',(#9982));
#2443=EDGE_LOOP('',(#9983));
#2444=EDGE_LOOP('',(#9984));
#2445=EDGE_LOOP('',(#9985));
#2446=EDGE_LOOP('',(#9986));
#2447=EDGE_LOOP('',(#9987));
#2448=EDGE_LOOP('',(#9988));
#2449=EDGE_LOOP('',(#9989));
#2450=EDGE_LOOP('',(#9990));
#2451=EDGE_LOOP('',(#9991,#9992,#9993,#9994));
#2452=EDGE_LOOP('',(#9995,#9996,#9997,#9998,#9999,#10000,#10001,#10002));
#2453=EDGE_LOOP('',(#10003,#10004,#10005,#10006,#10007,#10008,#10009,#10010));
#2454=EDGE_LOOP('',(#10011,#10012,#10013,#10014,#10015,#10016,#10017,#10018,
#10019,#10020,#10021,#10022,#10023,#10024,#10025,#10026,#10027,#10028,#10029,
#10030));
#2455=EDGE_LOOP('',(#10031,#10032,#10033,#10034,#10035,#10036,#10037,#10038,
#10039,#10040,#10041,#10042,#10043,#10044,#10045,#10046,#10047,#10048,#10049,
#10050));
#2456=EDGE_LOOP('',(#10051,#10052,#10053,#10054));
#2457=EDGE_LOOP('',(#10055,#10056,#10057,#10058));
#2458=EDGE_LOOP('',(#10059,#10060,#10061,#10062));
#2459=EDGE_LOOP('',(#10063,#10064,#10065,#10066));
#2460=EDGE_LOOP('',(#10067,#10068,#10069,#10070));
#2461=EDGE_LOOP('',(#10071,#10072,#10073,#10074));
#2462=EDGE_LOOP('',(#10075,#10076,#10077,#10078));
#2463=EDGE_LOOP('',(#10079,#10080,#10081,#10082,#10083,#10084,#10085,#10086));
#2464=EDGE_LOOP('',(#10087,#10088,#10089,#10090));
#2465=EDGE_LOOP('',(#10091,#10092,#10093,#10094));
#2466=EDGE_LOOP('',(#10095,#10096,#10097,#10098));
#2467=EDGE_LOOP('',(#10099,#10100,#10101,#10102));
#2468=EDGE_LOOP('',(#10103,#10104,#10105,#10106));
#2469=EDGE_LOOP('',(#10107,#10108,#10109,#10110));
#2470=EDGE_LOOP('',(#10111,#10112,#10113,#10114));
#2471=EDGE_LOOP('',(#10115,#10116,#10117,#10118,#10119,#10120,#10121,#10122));
#2472=EDGE_LOOP('',(#10123,#10124,#10125,#10126));
#2473=EDGE_LOOP('',(#10127,#10128,#10129,#10130));
#2474=EDGE_LOOP('',(#10131,#10132,#10133,#10134));
#2475=EDGE_LOOP('',(#10135,#10136,#10137,#10138));
#2476=EDGE_LOOP('',(#10139,#10140,#10141,#10142));
#2477=EDGE_LOOP('',(#10143,#10144,#10145,#10146));
#2478=EDGE_LOOP('',(#10147,#10148,#10149,#10150));
#2479=EDGE_LOOP('',(#10151,#10152,#10153,#10154));
#2480=EDGE_LOOP('',(#10155,#10156,#10157,#10158));
#2481=EDGE_LOOP('',(#10159,#10160,#10161,#10162));
#2482=EDGE_LOOP('',(#10163,#10164,#10165,#10166));
#2483=EDGE_LOOP('',(#10167,#10168,#10169,#10170));
#2484=EDGE_LOOP('',(#10171,#10172,#10173,#10174,#10175,#10176));
#2485=EDGE_LOOP('',(#10177,#10178,#10179,#10180,#10181));
#2486=EDGE_LOOP('',(#10182,#10183,#10184,#10185,#10186,#10187,#10188,#10189,
#10190));
#2487=EDGE_LOOP('',(#10191,#10192,#10193,#10194));
#2488=EDGE_LOOP('',(#10195,#10196,#10197,#10198,#10199));
#2489=EDGE_LOOP('',(#10200,#10201,#10202,#10203,#10204));
#2490=EDGE_LOOP('',(#10205));
#2491=EDGE_LOOP('',(#10206));
#2492=EDGE_LOOP('',(#10207));
#2493=EDGE_LOOP('',(#10208));
#2494=EDGE_LOOP('',(#10209,#10210,#10211,#10212));
#2495=EDGE_LOOP('',(#10213,#10214,#10215,#10216));
#2496=EDGE_LOOP('',(#10217,#10218,#10219,#10220));
#2497=EDGE_LOOP('',(#10221,#10222,#10223,#10224));
#2498=EDGE_LOOP('',(#10225,#10226,#10227,#10228,#10229,#10230));
#2499=EDGE_LOOP('',(#10231,#10232,#10233,#10234,#10235));
#2500=EDGE_LOOP('',(#10236,#10237,#10238,#10239,#10240,#10241,#10242,#10243,
#10244));
#2501=EDGE_LOOP('',(#10245,#10246,#10247,#10248));
#2502=EDGE_LOOP('',(#10249,#10250,#10251,#10252,#10253));
#2503=EDGE_LOOP('',(#10254,#10255,#10256,#10257,#10258));
#2504=EDGE_LOOP('',(#10259));
#2505=EDGE_LOOP('',(#10260));
#2506=EDGE_LOOP('',(#10261));
#2507=EDGE_LOOP('',(#10262));
#2508=EDGE_LOOP('',(#10263,#10264,#10265,#10266));
#2509=EDGE_LOOP('',(#10267,#10268,#10269,#10270));
#2510=EDGE_LOOP('',(#10271,#10272,#10273,#10274));
#2511=EDGE_LOOP('',(#10275,#10276,#10277,#10278));
#2512=EDGE_LOOP('',(#10279,#10280,#10281,#10282));
#2513=EDGE_LOOP('',(#10283,#10284,#10285,#10286));
#2514=EDGE_LOOP('',(#10287,#10288,#10289,#10290,#10291,#10292));
#2515=EDGE_LOOP('',(#10293,#10294,#10295,#10296,#10297));
#2516=EDGE_LOOP('',(#10298,#10299,#10300,#10301,#10302));
#2517=EDGE_LOOP('',(#10303,#10304,#10305,#10306,#10307));
#2518=EDGE_LOOP('',(#10308,#10309,#10310,#10311,#10312));
#2519=EDGE_LOOP('',(#10313,#10314,#10315,#10316));
#2520=EDGE_LOOP('',(#10317,#10318,#10319,#10320));
#2521=EDGE_LOOP('',(#10321,#10322,#10323,#10324));
#2522=EDGE_LOOP('',(#10325,#10326,#10327,#10328));
#2523=EDGE_LOOP('',(#10329,#10330,#10331,#10332));
#2524=EDGE_LOOP('',(#10333,#10334,#10335,#10336));
#2525=EDGE_LOOP('',(#10337,#10338,#10339,#10340,#10341,#10342));
#2526=EDGE_LOOP('',(#10343,#10344,#10345,#10346,#10347));
#2527=EDGE_LOOP('',(#10348,#10349,#10350,#10351,#10352));
#2528=EDGE_LOOP('',(#10353,#10354,#10355,#10356,#10357));
#2529=EDGE_LOOP('',(#10358,#10359,#10360,#10361,#10362));
#2530=EDGE_LOOP('',(#10363,#10364,#10365,#10366));
#2531=EDGE_LOOP('',(#10367,#10368,#10369,#10370));
#2532=EDGE_LOOP('',(#10371,#10372,#10373,#10374));
#2533=EDGE_LOOP('',(#10375,#10376,#10377,#10378));
#2534=EDGE_LOOP('',(#10379,#10380,#10381,#10382));
#2535=EDGE_LOOP('',(#10383,#10384,#10385,#10386));
#2536=EDGE_LOOP('',(#10387,#10388,#10389,#10390,#10391,#10392,#10393,#10394,
#10395,#10396,#10397,#10398));
#2537=EDGE_LOOP('',(#10399,#10400,#10401,#10402,#10403,#10404,#10405,#10406,
#10407,#10408,#10409,#10410,#10411,#10412,#10413,#10414));
#2538=EDGE_LOOP('',(#10415,#10416,#10417,#10418));
#2539=EDGE_LOOP('',(#10419,#10420,#10421,#10422));
#2540=EDGE_LOOP('',(#10423,#10424,#10425,#10426,#10427,#10428));
#2541=EDGE_LOOP('',(#10429));
#2542=EDGE_LOOP('',(#10430));
#2543=EDGE_LOOP('',(#10431,#10432,#10433,#10434));
#2544=EDGE_LOOP('',(#10435,#10436,#10437,#10438));
#2545=EDGE_LOOP('',(#10439,#10440,#10441,#10442));
#2546=EDGE_LOOP('',(#10443,#10444,#10445,#10446));
#2547=EDGE_LOOP('',(#10447,#10448,#10449,#10450,#10451,#10452));
#2548=EDGE_LOOP('',(#10453));
#2549=EDGE_LOOP('',(#10454));
#2550=EDGE_LOOP('',(#10455,#10456,#10457,#10458,#10459,#10460,#10461));
#2551=EDGE_LOOP('',(#10462));
#2552=EDGE_LOOP('',(#10463));
#2553=EDGE_LOOP('',(#10464,#10465,#10466,#10467));
#2554=EDGE_LOOP('',(#10468,#10469,#10470,#10471));
#2555=EDGE_LOOP('',(#10472,#10473,#10474,#10475));
#2556=EDGE_LOOP('',(#10476,#10477,#10478,#10479));
#2557=EDGE_LOOP('',(#10480,#10481,#10482,#10483,#10484,#10485));
#2558=EDGE_LOOP('',(#10486));
#2559=EDGE_LOOP('',(#10487));
#2560=EDGE_LOOP('',(#10488,#10489,#10490,#10491,#10492,#10493,#10494));
#2561=EDGE_LOOP('',(#10495));
#2562=EDGE_LOOP('',(#10496));
#2563=EDGE_LOOP('',(#10497,#10498,#10499,#10500));
#2564=EDGE_LOOP('',(#10501,#10502,#10503,#10504));
#2565=EDGE_LOOP('',(#10505,#10506,#10507,#10508,#10509,#10510,#10511,#10512));
#2566=EDGE_LOOP('',(#10513,#10514));
#2567=EDGE_LOOP('',(#10515,#10516));
#2568=EDGE_LOOP('',(#10517,#10518,#10519,#10520));
#2569=EDGE_LOOP('',(#10521,#10522,#10523,#10524,#10525,#10526));
#2570=EDGE_LOOP('',(#10527,#10528,#10529,#10530,#10531));
#2571=EDGE_LOOP('',(#10532,#10533,#10534,#10535,#10536));
#2572=EDGE_LOOP('',(#10537));
#2573=EDGE_LOOP('',(#10538));
#2574=EDGE_LOOP('',(#10539,#10540,#10541,#10542,#10543));
#2575=EDGE_LOOP('',(#10544,#10545,#10546,#10547,#10548));
#2576=EDGE_LOOP('',(#10549,#10550,#10551,#10552,#10553,#10554));
#2577=EDGE_LOOP('',(#10555,#10556,#10557,#10558));
#2578=EDGE_LOOP('',(#10559));
#2579=EDGE_LOOP('',(#10560));
#2580=EDGE_LOOP('',(#10561));
#2581=EDGE_LOOP('',(#10562));
#2582=EDGE_LOOP('',(#10563,#10564,#10565,#10566));
#2583=EDGE_LOOP('',(#10567,#10568,#10569,#10570,#10571));
#2584=EDGE_LOOP('',(#10572,#10573,#10574,#10575,#10576));
#2585=EDGE_LOOP('',(#10577));
#2586=EDGE_LOOP('',(#10578));
#2587=EDGE_LOOP('',(#10579,#10580,#10581,#10582,#10583));
#2588=EDGE_LOOP('',(#10584,#10585,#10586,#10587));
#2589=EDGE_LOOP('',(#10588,#10589,#10590,#10591,#10592));
#2590=EDGE_LOOP('',(#10593,#10594,#10595,#10596));
#2591=EDGE_LOOP('',(#10597,#10598,#10599,#10600,#10601));
#2592=EDGE_LOOP('',(#10602,#10603,#10604,#10605,#10606));
#2593=EDGE_LOOP('',(#10607,#10608,#10609,#10610));
#2594=EDGE_LOOP('',(#10611,#10612,#10613,#10614));
#2595=EDGE_LOOP('',(#10615,#10616,#10617,#10618));
#2596=EDGE_LOOP('',(#10619,#10620,#10621,#10622));
#2597=EDGE_LOOP('',(#10623,#10624,#10625,#10626,#10627,#10628));
#2598=EDGE_LOOP('',(#10629,#10630,#10631,#10632,#10633,#10634));
#2599=EDGE_LOOP('',(#10635));
#2600=EDGE_LOOP('',(#10636));
#2601=EDGE_LOOP('',(#10637));
#2602=EDGE_LOOP('',(#10638));
#2603=EDGE_LOOP('',(#10639));
#2604=EDGE_LOOP('',(#10640));
#2605=EDGE_LOOP('',(#10641));
#2606=EDGE_LOOP('',(#10642));
#2607=EDGE_LOOP('',(#10643));
#2608=EDGE_LOOP('',(#10644));
#2609=EDGE_LOOP('',(#10645));
#2610=EDGE_LOOP('',(#10646));
#2611=EDGE_LOOP('',(#10647,#10648,#10649,#10650,#10651));
#2612=EDGE_LOOP('',(#10652,#10653,#10654,#10655));
#2613=EDGE_LOOP('',(#10656,#10657,#10658,#10659,#10660));
#2614=EDGE_LOOP('',(#10661,#10662,#10663,#10664));
#2615=EDGE_LOOP('',(#10665,#10666,#10667,#10668,#10669));
#2616=EDGE_LOOP('',(#10670,#10671,#10672,#10673,#10674));
#2617=EDGE_LOOP('',(#10675,#10676,#10677,#10678));
#2618=EDGE_LOOP('',(#10679,#10680,#10681,#10682));
#2619=EDGE_LOOP('',(#10683,#10684,#10685,#10686));
#2620=EDGE_LOOP('',(#10687,#10688,#10689,#10690));
#2621=EDGE_LOOP('',(#10691,#10692,#10693,#10694,#10695,#10696));
#2622=EDGE_LOOP('',(#10697,#10698,#10699,#10700,#10701,#10702));
#2623=EDGE_LOOP('',(#10703));
#2624=EDGE_LOOP('',(#10704));
#2625=EDGE_LOOP('',(#10705));
#2626=EDGE_LOOP('',(#10706));
#2627=EDGE_LOOP('',(#10707));
#2628=EDGE_LOOP('',(#10708));
#2629=EDGE_LOOP('',(#10709));
#2630=EDGE_LOOP('',(#10710));
#2631=EDGE_LOOP('',(#10711));
#2632=EDGE_LOOP('',(#10712));
#2633=EDGE_LOOP('',(#10713));
#2634=EDGE_LOOP('',(#10714));
#2635=EDGE_LOOP('',(#10715,#10716,#10717,#10718));
#2636=EDGE_LOOP('',(#10719,#10720,#10721,#10722,#10723));
#2637=EDGE_LOOP('',(#10724,#10725,#10726,#10727,#10728));
#2638=EDGE_LOOP('',(#10729));
#2639=EDGE_LOOP('',(#10730));
#2640=EDGE_LOOP('',(#10731,#10732,#10733,#10734));
#2641=EDGE_LOOP('',(#10735,#10736,#10737,#10738));
#2642=EDGE_LOOP('',(#10739,#10740,#10741,#10742));
#2643=EDGE_LOOP('',(#10743,#10744,#10745,#10746));
#2644=EDGE_LOOP('',(#10747,#10748,#10749,#10750));
#2645=EDGE_LOOP('',(#10751,#10752,#10753,#10754));
#2646=EDGE_LOOP('',(#10755,#10756,#10757,#10758));
#2647=EDGE_LOOP('',(#10759,#10760,#10761,#10762));
#2648=EDGE_LOOP('',(#10763,#10764,#10765,#10766));
#2649=EDGE_LOOP('',(#10767,#10768,#10769,#10770));
#2650=EDGE_LOOP('',(#10771,#10772,#10773,#10774));
#2651=EDGE_LOOP('',(#10775,#10776,#10777,#10778));
#2652=EDGE_LOOP('',(#10779,#10780,#10781,#10782));
#2653=EDGE_LOOP('',(#10783,#10784,#10785,#10786,#10787,#10788,#10789,#10790));
#2654=EDGE_LOOP('',(#10791,#10792,#10793,#10794));
#2655=EDGE_LOOP('',(#10795,#10796,#10797,#10798));
#2656=EDGE_LOOP('',(#10799,#10800,#10801,#10802));
#2657=EDGE_LOOP('',(#10803,#10804,#10805,#10806));
#2658=EDGE_LOOP('',(#10807,#10808,#10809,#10810));
#2659=EDGE_LOOP('',(#10811,#10812,#10813,#10814));
#2660=EDGE_LOOP('',(#10815,#10816,#10817,#10818));
#2661=EDGE_LOOP('',(#10819,#10820,#10821,#10822));
#2662=EDGE_LOOP('',(#10823,#10824,#10825,#10826));
#2663=EDGE_LOOP('',(#10827,#10828,#10829,#10830));
#2664=EDGE_LOOP('',(#10831,#10832,#10833,#10834));
#2665=EDGE_LOOP('',(#10835,#10836,#10837,#10838));
#2666=EDGE_LOOP('',(#10839,#10840,#10841,#10842,#10843,#10844,#10845));
#2667=EDGE_LOOP('',(#10846,#10847,#10848,#10849));
#2668=EDGE_LOOP('',(#10850,#10851,#10852,#10853));
#2669=EDGE_LOOP('',(#10854,#10855,#10856,#10857,#10858,#10859,#10860,#10861));
#2670=EDGE_LOOP('',(#10862,#10863,#10864,#10865,#10866));
#2671=EDGE_LOOP('',(#10867,#10868,#10869));
#2672=EDGE_LOOP('',(#10870,#10871,#10872,#10873));
#2673=EDGE_LOOP('',(#10874));
#2674=EDGE_LOOP('',(#10875,#10876,#10877,#10878));
#2675=EDGE_LOOP('',(#10879));
#2676=EDGE_LOOP('',(#10880,#10881,#10882));
#2677=EDGE_LOOP('',(#10883,#10884,#10885,#10886));
#2678=EDGE_LOOP('',(#10887));
#2679=EDGE_LOOP('',(#10888,#10889,#10890,#10891));
#2680=EDGE_LOOP('',(#10892));
#2681=EDGE_LOOP('',(#10893,#10894,#10895,#10896));
#2682=EDGE_LOOP('',(#10897,#10898,#10899,#10900,#10901,#10902));
#2683=EDGE_LOOP('',(#10903,#10904,#10905,#10906,#10907,#10908,#10909));
#2684=EDGE_LOOP('',(#10910,#10911,#10912,#10913,#10914,#10915));
#2685=EDGE_LOOP('',(#10916,#10917,#10918,#10919,#10920,#10921));
#2686=EDGE_LOOP('',(#10922,#10923,#10924,#10925));
#2687=EDGE_LOOP('',(#10926,#10927,#10928,#10929));
#2688=EDGE_LOOP('',(#10930,#10931,#10932,#10933,#10934,#10935));
#2689=EDGE_LOOP('',(#10936,#10937,#10938,#10939,#10940,#10941));
#2690=EDGE_LOOP('',(#10942));
#2691=EDGE_LOOP('',(#10943));
#2692=EDGE_LOOP('',(#10944));
#2693=EDGE_LOOP('',(#10945,#10946,#10947,#10948));
#2694=EDGE_LOOP('',(#10949,#10950,#10951,#10952,#10953,#10954,#10955,#10956,
#10957,#10958,#10959,#10960,#10961,#10962,#10963,#10964,#10965,#10966,#10967,
#10968,#10969,#10970,#10971,#10972,#10973,#10974,#10975,#10976,#10977,#10978));
#2695=EDGE_LOOP('',(#10979,#10980,#10981,#10982));
#2696=EDGE_LOOP('',(#10983,#10984,#10985,#10986,#10987,#10988,#10989,#10990,
#10991,#10992,#10993,#10994,#10995,#10996,#10997,#10998,#10999,#11000,#11001,
#11002,#11003,#11004,#11005,#11006,#11007,#11008,#11009,#11010,#11011,#11012));
#2697=EDGE_LOOP('',(#11013,#11014,#11015,#11016,#11017,#11018,#11019));
#2698=EDGE_LOOP('',(#11020,#11021,#11022,#11023,#11024,#11025,#11026));
#2699=EDGE_LOOP('',(#11027,#11028,#11029,#11030));
#2700=EDGE_LOOP('',(#11031,#11032,#11033,#11034));
#2701=EDGE_LOOP('',(#11035,#11036,#11037,#11038));
#2702=EDGE_LOOP('',(#11039,#11040,#11041,#11042));
#2703=EDGE_LOOP('',(#11043,#11044,#11045,#11046));
#2704=EDGE_LOOP('',(#11047,#11048,#11049,#11050));
#2705=EDGE_LOOP('',(#11051,#11052,#11053,#11054));
#2706=EDGE_LOOP('',(#11055,#11056,#11057,#11058));
#2707=EDGE_LOOP('',(#11059,#11060,#11061,#11062));
#2708=EDGE_LOOP('',(#11063,#11064,#11065,#11066));
#2709=EDGE_LOOP('',(#11067,#11068,#11069,#11070,#11071,#11072,#11073,#11074));
#2710=EDGE_LOOP('',(#11075,#11076,#11077,#11078));
#2711=EDGE_LOOP('',(#11079,#11080,#11081,#11082));
#2712=EDGE_LOOP('',(#11083,#11084,#11085,#11086));
#2713=EDGE_LOOP('',(#11087,#11088,#11089,#11090));
#2714=EDGE_LOOP('',(#11091,#11092,#11093,#11094));
#2715=EDGE_LOOP('',(#11095,#11096,#11097,#11098));
#2716=EDGE_LOOP('',(#11099,#11100,#11101,#11102));
#2717=EDGE_LOOP('',(#11103,#11104,#11105,#11106));
#2718=EDGE_LOOP('',(#11107,#11108,#11109,#11110));
#2719=EDGE_LOOP('',(#11111,#11112,#11113,#11114,#11115,#11116,#11117,#11118,
#11119,#11120,#11121,#11122));
#2720=EDGE_LOOP('',(#11123,#11124,#11125,#11126));
#2721=EDGE_LOOP('',(#11127));
#2722=EDGE_LOOP('',(#11128,#11129,#11130,#11131,#11132,#11133));
#2723=EDGE_LOOP('',(#11134));
#2724=EDGE_LOOP('',(#11135));
#2725=EDGE_LOOP('',(#11136,#11137,#11138,#11139,#11140,#11141));
#2726=EDGE_LOOP('',(#11142,#11143,#11144,#11145,#11146,#11147));
#2727=EDGE_LOOP('',(#11148,#11149,#11150,#11151,#11152,#11153));
#2728=EDGE_LOOP('',(#11154,#11155,#11156,#11157,#11158,#11159));
#2729=EDGE_LOOP('',(#11160,#11161,#11162,#11163,#11164,#11165));
#2730=EDGE_LOOP('',(#11166,#11167,#11168,#11169,#11170,#11171));
#2731=EDGE_LOOP('',(#11172,#11173,#11174,#11175));
#2732=EDGE_LOOP('',(#11176,#11177,#11178,#11179));
#2733=EDGE_LOOP('',(#11180,#11181,#11182,#11183,#11184,#11185,#11186,#11187,
#11188,#11189,#11190,#11191,#11192,#11193,#11194,#11195,#11196,#11197,#11198,
#11199));
#2734=EDGE_LOOP('',(#11200,#11201,#11202,#11203,#11204,#11205,#11206,#11207,
#11208,#11209,#11210,#11211,#11212,#11213,#11214,#11215,#11216,#11217,#11218,
#11219,#11220));
#2735=EDGE_LOOP('',(#11221,#11222,#11223));
#2736=EDGE_LOOP('',(#11224,#11225,#11226));
#2737=EDGE_LOOP('',(#11227,#11228,#11229));
#2738=EDGE_LOOP('',(#11230,#11231,#11232));
#2739=EDGE_LOOP('',(#11233,#11234,#11235));
#2740=EDGE_LOOP('',(#11236,#11237,#11238));
#2741=EDGE_LOOP('',(#11239,#11240,#11241,#11242));
#2742=EDGE_LOOP('',(#11243,#11244,#11245,#11246,#11247));
#2743=EDGE_LOOP('',(#11248,#11249,#11250,#11251));
#2744=EDGE_LOOP('',(#11252,#11253,#11254,#11255,#11256));
#2745=EDGE_LOOP('',(#11257));
#2746=EDGE_LOOP('',(#11258));
#2747=EDGE_LOOP('',(#11259));
#2748=EDGE_LOOP('',(#11260));
#2749=EDGE_LOOP('',(#11261,#11262,#11263,#11264));
#2750=EDGE_LOOP('',(#11265,#11266,#11267,#11268,#11269));
#2751=EDGE_LOOP('',(#11270,#11271,#11272,#11273,#11274));
#2752=EDGE_LOOP('',(#11275));
#2753=EDGE_LOOP('',(#11276));
#2754=LINE('',#17426,#3574);
#2755=LINE('',#17432,#3575);
#2756=LINE('',#17438,#3576);
#2757=LINE('',#17444,#3577);
#2758=LINE('',#17450,#3578);
#2759=LINE('',#17456,#3579);
#2760=LINE('',#17463,#3580);
#2761=LINE('',#17479,#3581);
#2762=LINE('',#17570,#3582);
#2763=LINE('',#17576,#3583);
#2764=LINE('',#17591,#3584);
#2765=LINE('',#17594,#3585);
#2766=LINE('',#17596,#3586);
#2767=LINE('',#17610,#3587);
#2768=LINE('',#17613,#3588);
#2769=LINE('',#17616,#3589);
#2770=LINE('',#17619,#3590);
#2771=LINE('',#17625,#3591);
#2772=LINE('',#17631,#3592);
#2773=LINE('',#17637,#3593);
#2774=LINE('',#17640,#3594);
#2775=LINE('',#17642,#3595);
#2776=LINE('',#17656,#3596);
#2777=LINE('',#17659,#3597);
#2778=LINE('',#17665,#3598);
#2779=LINE('',#17671,#3599);
#2780=LINE('',#17677,#3600);
#2781=LINE('',#17680,#3601);
#2782=LINE('',#17685,#3602);
#2783=LINE('',#17689,#3603);
#2784=LINE('',#17692,#3604);
#2785=LINE('',#17697,#3605);
#2786=LINE('',#17702,#3606);
#2787=LINE('',#17704,#3607);
#2788=LINE('',#17706,#3608);
#2789=LINE('',#17709,#3609);
#2790=LINE('',#17713,#3610);
#2791=LINE('',#17715,#3611);
#2792=LINE('',#17717,#3612);
#2793=LINE('',#17718,#3613);
#2794=LINE('',#17721,#3614);
#2795=LINE('',#17723,#3615);
#2796=LINE('',#17725,#3616);
#2797=LINE('',#17726,#3617);
#2798=LINE('',#17730,#3618);
#2799=LINE('',#17732,#3619);
#2800=LINE('',#17734,#3620);
#2801=LINE('',#17736,#3621);
#2802=LINE('',#17741,#3622);
#2803=LINE('',#17743,#3623);
#2804=LINE('',#17745,#3624);
#2805=LINE('',#17746,#3625);
#2806=LINE('',#17750,#3626);
#2807=LINE('',#17752,#3627);
#2808=LINE('',#17754,#3628);
#2809=LINE('',#17757,#3629);
#2810=LINE('',#17763,#3630);
#2811=LINE('',#17769,#3631);
#2812=LINE('',#17781,#3632);
#2813=LINE('',#17783,#3633);
#2814=LINE('',#17785,#3634);
#2815=LINE('',#17789,#3635);
#2816=LINE('',#17794,#3636);
#2817=LINE('',#17796,#3637);
#2818=LINE('',#17798,#3638);
#2819=LINE('',#17799,#3639);
#2820=LINE('',#17802,#3640);
#2821=LINE('',#17804,#3641);
#2822=LINE('',#17805,#3642);
#2823=LINE('',#17807,#3643);
#2824=LINE('',#17809,#3644);
#2825=LINE('',#17810,#3645);
#2826=LINE('',#17815,#3646);
#2827=LINE('',#17820,#3647);
#2828=LINE('',#17825,#3648);
#2829=LINE('',#17827,#3649);
#2830=LINE('',#17828,#3650);
#2831=LINE('',#17831,#3651);
#2832=LINE('',#17833,#3652);
#2833=LINE('',#17834,#3653);
#2834=LINE('',#17837,#3654);
#2835=LINE('',#17838,#3655);
#2836=LINE('',#17842,#3656);
#2837=LINE('',#17843,#3657);
#2838=LINE('',#17849,#3658);
#2839=LINE('',#17854,#3659);
#2840=LINE('',#17857,#3660);
#2841=LINE('',#17859,#3661);
#2842=LINE('',#17860,#3662);
#2843=LINE('',#17862,#3663);
#2844=LINE('',#17866,#3664);
#2845=LINE('',#17870,#3665);
#2846=LINE('',#17872,#3666);
#2847=LINE('',#17877,#3667);
#2848=LINE('',#17881,#3668);
#2849=LINE('',#17886,#3669);
#2850=LINE('',#17890,#3670);
#2851=LINE('',#17894,#3671);
#2852=LINE('',#17901,#3672);
#2853=LINE('',#17905,#3673);
#2854=LINE('',#17910,#3674);
#2855=LINE('',#17911,#3675);
#2856=LINE('',#17912,#3676);
#2857=LINE('',#17916,#3677);
#2858=LINE('',#17918,#3678);
#2859=LINE('',#17920,#3679);
#2860=LINE('',#17921,#3680);
#2861=LINE('',#17926,#3681);
#2862=LINE('',#17932,#3682);
#2863=LINE('',#17936,#3683);
#2864=LINE('',#17940,#3684);
#2865=LINE('',#17944,#3685);
#2866=LINE('',#17948,#3686);
#2867=LINE('',#17950,#3687);
#2868=LINE('',#17955,#3688);
#2869=LINE('',#17958,#3689);
#2870=LINE('',#17962,#3690);
#2871=LINE('',#17965,#3691);
#2872=LINE('',#17966,#3692);
#2873=LINE('',#17968,#3693);
#2874=LINE('',#17969,#3694);
#2875=LINE('',#17971,#3695);
#2876=LINE('',#17972,#3696);
#2877=LINE('',#17974,#3697);
#2878=LINE('',#17975,#3698);
#2879=LINE('',#17977,#3699);
#2880=LINE('',#17978,#3700);
#2881=LINE('',#17983,#3701);
#2882=LINE('',#17984,#3702);
#2883=LINE('',#17986,#3703);
#2884=LINE('',#17990,#3704);
#2885=LINE('',#17994,#3705);
#2886=LINE('',#17996,#3706);
#2887=LINE('',#18000,#3707);
#2888=LINE('',#18006,#3708);
#2889=LINE('',#18007,#3709);
#2890=LINE('',#18011,#3710);
#2891=LINE('',#18012,#3711);
#2892=LINE('',#18013,#3712);
#2893=LINE('',#18016,#3713);
#2894=LINE('',#18020,#3714);
#2895=LINE('',#18023,#3715);
#2896=LINE('',#18027,#3716);
#2897=LINE('',#18031,#3717);
#2898=LINE('',#18032,#3718);
#2899=LINE('',#18036,#3719);
#2900=LINE('',#18038,#3720);
#2901=LINE('',#18039,#3721);
#2902=LINE('',#18043,#3722);
#2903=LINE('',#18047,#3723);
#2904=LINE('',#18048,#3724);
#2905=LINE('',#18052,#3725);
#2906=LINE('',#18054,#3726);
#2907=LINE('',#18056,#3727);
#2908=LINE('',#18057,#3728);
#2909=LINE('',#18060,#3729);
#2910=LINE('',#18077,#3730);
#2911=LINE('',#18079,#3731);
#2912=LINE('',#18081,#3732);
#2913=LINE('',#18082,#3733);
#2914=LINE('',#18086,#3734);
#2915=LINE('',#18088,#3735);
#2916=LINE('',#18090,#3736);
#2917=LINE('',#18095,#3737);
#2918=LINE('',#18097,#3738);
#2919=LINE('',#18101,#3739);
#2920=LINE('',#18103,#3740);
#2921=LINE('',#18106,#3741);
#2922=LINE('',#18109,#3742);
#2923=LINE('',#18110,#3743);
#2924=LINE('',#18115,#3744);
#2925=LINE('',#18116,#3745);
#2926=LINE('',#18124,#3746);
#2927=LINE('',#18126,#3747);
#2928=LINE('',#18127,#3748);
#2929=LINE('',#18130,#3749);
#2930=LINE('',#18131,#3750);
#2931=LINE('',#18134,#3751);
#2932=LINE('',#18135,#3752);
#2933=LINE('',#18139,#3753);
#2934=LINE('',#18140,#3754);
#2935=LINE('',#18141,#3755);
#2936=LINE('',#18146,#3756);
#2937=LINE('',#18152,#3757);
#2938=LINE('',#18157,#3758);
#2939=LINE('',#18158,#3759);
#2940=LINE('',#18161,#3760);
#2941=LINE('',#18163,#3761);
#2942=LINE('',#18165,#3762);
#2943=LINE('',#18170,#3763);
#2944=LINE('',#18171,#3764);
#2945=LINE('',#18174,#3765);
#2946=LINE('',#18176,#3766);
#2947=LINE('',#18177,#3767);
#2948=LINE('',#18187,#3768);
#2949=LINE('',#18189,#3769);
#2950=LINE('',#18190,#3770);
#2951=LINE('',#18193,#3771);
#2952=LINE('',#18194,#3772);
#2953=LINE('',#18199,#3773);
#2954=LINE('',#18201,#3774);
#2955=LINE('',#18202,#3775);
#2956=LINE('',#18205,#3776);
#2957=LINE('',#18206,#3777);
#2958=LINE('',#18209,#3778);
#2959=LINE('',#18221,#3779);
#2960=LINE('',#18223,#3780);
#2961=LINE('',#18225,#3781);
#2962=LINE('',#18226,#3782);
#2963=LINE('',#18232,#3783);
#2964=LINE('',#18234,#3784);
#2965=LINE('',#18236,#3785);
#2966=LINE('',#18237,#3786);
#2967=LINE('',#18242,#3787);
#2968=LINE('',#18247,#3788);
#2969=LINE('',#18252,#3789);
#2970=LINE('',#18257,#3790);
#2971=LINE('',#18477,#3791);
#2972=LINE('',#18480,#3792);
#2973=LINE('',#18483,#3793);
#2974=LINE('',#18487,#3794);
#2975=LINE('',#18489,#3795);
#2976=LINE('',#18493,#3796);
#2977=LINE('',#18495,#3797);
#2978=LINE('',#18499,#3798);
#2979=LINE('',#18503,#3799);
#2980=LINE('',#18511,#3800);
#2981=LINE('',#18512,#3801);
#2982=LINE('',#18518,#3802);
#2983=LINE('',#18521,#3803);
#2984=LINE('',#18524,#3804);
#2985=LINE('',#18528,#3805);
#2986=LINE('',#18530,#3806);
#2987=LINE('',#18534,#3807);
#2988=LINE('',#18536,#3808);
#2989=LINE('',#18540,#3809);
#2990=LINE('',#18542,#3810);
#2991=LINE('',#18544,#3811);
#2992=LINE('',#18548,#3812);
#2993=LINE('',#18558,#3813);
#2994=LINE('',#18559,#3814);
#2995=LINE('',#18563,#3815);
#2996=LINE('',#18566,#3816);
#2997=LINE('',#18567,#3817);
#2998=LINE('',#18571,#3818);
#2999=LINE('',#18574,#3819);
#3000=LINE('',#18575,#3820);
#3001=LINE('',#18578,#3821);
#3002=LINE('',#18588,#3822);
#3003=LINE('',#18593,#3823);
#3004=LINE('',#18597,#3824);
#3005=LINE('',#18601,#3825);
#3006=LINE('',#18603,#3826);
#3007=LINE('',#18611,#3827);
#3008=LINE('',#18613,#3828);
#3009=LINE('',#18622,#3829);
#3010=LINE('',#18630,#3830);
#3011=LINE('',#18655,#3831);
#3012=LINE('',#18657,#3832);
#3013=LINE('',#18661,#3833);
#3014=LINE('',#18663,#3834);
#3015=LINE('',#18666,#3835);
#3016=LINE('',#18670,#3836);
#3017=LINE('',#18674,#3837);
#3018=LINE('',#18679,#3838);
#3019=LINE('',#18682,#3839);
#3020=LINE('',#18683,#3840);
#3021=LINE('',#18687,#3841);
#3022=LINE('',#18689,#3842);
#3023=LINE('',#18691,#3843);
#3024=LINE('',#18692,#3844);
#3025=LINE('',#18704,#3845);
#3026=LINE('',#18715,#3846);
#3027=LINE('',#18717,#3847);
#3028=LINE('',#18720,#3848);
#3029=LINE('',#18724,#3849);
#3030=LINE('',#18736,#3850);
#3031=LINE('',#18739,#3851);
#3032=LINE('',#18740,#3852);
#3033=LINE('',#18752,#3853);
#3034=LINE('',#18755,#3854);
#3035=LINE('',#18756,#3855);
#3036=LINE('',#18759,#3856);
#3037=LINE('',#18760,#3857);
#3038=LINE('',#18762,#3858);
#3039=LINE('',#18764,#3859);
#3040=LINE('',#18765,#3860);
#3041=LINE('',#18767,#3861);
#3042=LINE('',#18772,#3862);
#3043=LINE('',#18774,#3863);
#3044=LINE('',#18775,#3864);
#3045=LINE('',#18795,#3865);
#3046=LINE('',#18801,#3866);
#3047=LINE('',#18809,#3867);
#3048=LINE('',#18814,#3868);
#3049=LINE('',#18816,#3869);
#3050=LINE('',#18824,#3870);
#3051=LINE('',#18830,#3871);
#3052=LINE('',#18837,#3872);
#3053=LINE('',#18843,#3873);
#3054=LINE('',#18845,#3874);
#3055=LINE('',#18859,#3875);
#3056=LINE('',#18940,#3876);
#3057=LINE('',#18984,#3877);
#3058=LINE('',#18987,#3878);
#3059=LINE('',#18989,#3879);
#3060=LINE('',#18994,#3880);
#3061=LINE('',#18999,#3881);
#3062=LINE('',#19001,#3882);
#3063=LINE('',#19006,#3883);
#3064=LINE('',#19011,#3884);
#3065=LINE('',#19015,#3885);
#3066=LINE('',#19016,#3886);
#3067=LINE('',#19018,#3887);
#3068=LINE('',#19020,#3888);
#3069=LINE('',#19022,#3889);
#3070=LINE('',#19027,#3890);
#3071=LINE('',#19029,#3891);
#3072=LINE('',#19031,#3892);
#3073=LINE('',#19049,#3893);
#3074=LINE('',#19068,#3894);
#3075=LINE('',#19073,#3895);
#3076=LINE('',#19104,#3896);
#3077=LINE('',#19120,#3897);
#3078=LINE('',#19125,#3898);
#3079=LINE('',#19130,#3899);
#3080=LINE('',#19136,#3900);
#3081=LINE('',#19143,#3901);
#3082=LINE('',#19146,#3902);
#3083=LINE('',#19151,#3903);
#3084=LINE('',#19158,#3904);
#3085=LINE('',#19161,#3905);
#3086=LINE('',#19164,#3906);
#3087=LINE('',#19168,#3907);
#3088=LINE('',#19171,#3908);
#3089=LINE('',#19174,#3909);
#3090=LINE('',#19175,#3910);
#3091=LINE('',#19180,#3911);
#3092=LINE('',#19183,#3912);
#3093=LINE('',#19186,#3913);
#3094=LINE('',#19188,#3914);
#3095=LINE('',#19189,#3915);
#3096=LINE('',#19192,#3916);
#3097=LINE('',#19194,#3917);
#3098=LINE('',#19195,#3918);
#3099=LINE('',#19198,#3919);
#3100=LINE('',#19202,#3920);
#3101=LINE('',#19204,#3921);
#3102=LINE('',#19206,#3922);
#3103=LINE('',#19209,#3923);
#3104=LINE('',#19213,#3924);
#3105=LINE('',#19218,#3925);
#3106=LINE('',#19219,#3926);
#3107=LINE('',#19223,#3927);
#3108=LINE('',#19225,#3928);
#3109=LINE('',#19227,#3929);
#3110=LINE('',#19228,#3930);
#3111=LINE('',#19232,#3931);
#3112=LINE('',#19233,#3932);
#3113=LINE('',#19237,#3933);
#3114=LINE('',#19239,#3934);
#3115=LINE('',#19240,#3935);
#3116=LINE('',#19242,#3936);
#3117=LINE('',#19244,#3937);
#3118=LINE('',#19245,#3938);
#3119=LINE('',#19248,#3939);
#3120=LINE('',#19249,#3940);
#3121=LINE('',#19252,#3941);
#3122=LINE('',#19253,#3942);
#3123=LINE('',#19257,#3943);
#3124=LINE('',#19258,#3944);
#3125=LINE('',#19262,#3945);
#3126=LINE('',#19264,#3946);
#3127=LINE('',#19265,#3947);
#3128=LINE('',#19267,#3948);
#3129=LINE('',#19269,#3949);
#3130=LINE('',#19270,#3950);
#3131=LINE('',#19271,#3951);
#3132=LINE('',#19275,#3952);
#3133=LINE('',#19276,#3953);
#3134=LINE('',#19284,#3954);
#3135=LINE('',#19285,#3955);
#3136=LINE('',#19300,#3956);
#3137=LINE('',#19308,#3957);
#3138=LINE('',#19311,#3958);
#3139=LINE('',#19318,#3959);
#3140=LINE('',#19326,#3960);
#3141=LINE('',#19329,#3961);
#3142=LINE('',#19340,#3962);
#3143=LINE('',#19346,#3963);
#3144=LINE('',#19351,#3964);
#3145=LINE('',#19355,#3965);
#3146=LINE('',#19359,#3966);
#3147=LINE('',#19363,#3967);
#3148=LINE('',#19368,#3968);
#3149=LINE('',#19372,#3969);
#3150=LINE('',#19376,#3970);
#3151=LINE('',#19380,#3971);
#3152=LINE('',#19383,#3972);
#3153=LINE('',#19384,#3973);
#3154=LINE('',#19386,#3974);
#3155=LINE('',#19387,#3975);
#3156=LINE('',#19389,#3976);
#3157=LINE('',#19390,#3977);
#3158=LINE('',#19392,#3978);
#3159=LINE('',#19393,#3979);
#3160=LINE('',#19422,#3980);
#3161=LINE('',#19462,#3981);
#3162=LINE('',#19468,#3982);
#3163=LINE('',#19474,#3983);
#3164=LINE('',#19480,#3984);
#3165=LINE('',#19489,#3985);
#3166=LINE('',#19495,#3986);
#3167=LINE('',#19504,#3987);
#3168=LINE('',#19511,#3988);
#3169=LINE('',#19516,#3989);
#3170=LINE('',#19533,#3990);
#3171=LINE('',#19536,#3991);
#3172=LINE('',#19541,#3992);
#3173=LINE('',#19547,#3993);
#3174=LINE('',#19553,#3994);
#3175=LINE('',#19559,#3995);
#3176=LINE('',#19573,#3996);
#3177=LINE('',#19589,#3997);
#3178=LINE('',#19682,#3998);
#3179=LINE('',#19758,#3999);
#3180=LINE('',#19842,#4000);
#3181=LINE('',#19935,#4001);
#3182=LINE('',#19937,#4002);
#3183=LINE('',#19939,#4003);
#3184=LINE('',#19940,#4004);
#3185=LINE('',#19944,#4005);
#3186=LINE('',#20040,#4006);
#3187=LINE('',#20041,#4007);
#3188=LINE('',#20042,#4008);
#3189=LINE('',#20057,#4009);
#3190=LINE('',#20059,#4010);
#3191=LINE('',#20061,#4011);
#3192=LINE('',#20063,#4012);
#3193=LINE('',#20065,#4013);
#3194=LINE('',#20066,#4014);
#3195=LINE('',#20069,#4015);
#3196=LINE('',#20071,#4016);
#3197=LINE('',#20072,#4017);
#3198=LINE('',#20075,#4018);
#3199=LINE('',#20076,#4019);
#3200=LINE('',#20079,#4020);
#3201=LINE('',#20080,#4021);
#3202=LINE('',#20083,#4022);
#3203=LINE('',#20084,#4023);
#3204=LINE('',#20087,#4024);
#3205=LINE('',#20088,#4025);
#3206=LINE('',#20090,#4026);
#3207=LINE('',#20094,#4027);
#3208=LINE('',#20096,#4028);
#3209=LINE('',#20098,#4029);
#3210=LINE('',#20100,#4030);
#3211=LINE('',#20102,#4031);
#3212=LINE('',#20103,#4032);
#3213=LINE('',#20107,#4033);
#3214=LINE('',#20109,#4034);
#3215=LINE('',#20111,#4035);
#3216=LINE('',#20113,#4036);
#3217=LINE('',#20114,#4037);
#3218=LINE('',#20116,#4038);
#3219=LINE('',#20117,#4039);
#3220=LINE('',#20119,#4040);
#3221=LINE('',#20121,#4041);
#3222=LINE('',#20123,#4042);
#3223=LINE('',#20124,#4043);
#3224=LINE('',#20125,#4044);
#3225=LINE('',#20127,#4045);
#3226=LINE('',#20129,#4046);
#3227=LINE('',#20133,#4047);
#3228=LINE('',#20136,#4048);
#3229=LINE('',#20139,#4049);
#3230=LINE('',#20140,#4050);
#3231=LINE('',#20143,#4051);
#3232=LINE('',#20146,#4052);
#3233=LINE('',#20149,#4053);
#3234=LINE('',#20150,#4054);
#3235=LINE('',#20153,#4055);
#3236=LINE('',#20154,#4056);
#3237=LINE('',#20157,#4057);
#3238=LINE('',#20158,#4058);
#3239=LINE('',#20161,#4059);
#3240=LINE('',#20162,#4060);
#3241=LINE('',#20165,#4061);
#3242=LINE('',#20166,#4062);
#3243=LINE('',#20169,#4063);
#3244=LINE('',#20170,#4064);
#3245=LINE('',#20173,#4065);
#3246=LINE('',#20176,#4066);
#3247=LINE('',#20177,#4067);
#3248=LINE('',#20180,#4068);
#3249=LINE('',#20182,#4069);
#3250=LINE('',#20187,#4070);
#3251=LINE('',#20190,#4071);
#3252=LINE('',#20194,#4072);
#3253=LINE('',#20196,#4073);
#3254=LINE('',#20199,#4074);
#3255=LINE('',#20202,#4075);
#3256=LINE('',#20207,#4076);
#3257=LINE('',#20217,#4077);
#3258=LINE('',#20219,#4078);
#3259=LINE('',#20222,#4079);
#3260=LINE('',#20223,#4080);
#3261=LINE('',#20226,#4081);
#3262=LINE('',#20227,#4082);
#3263=LINE('',#20229,#4083);
#3264=LINE('',#20231,#4084);
#3265=LINE('',#20245,#4085);
#3266=LINE('',#20247,#4086);
#3267=LINE('',#20332,#4087);
#3268=LINE('',#20424,#4088);
#3269=LINE('',#21148,#4089);
#3270=LINE('',#21181,#4090);
#3271=LINE('',#21204,#4091);
#3272=LINE('',#21243,#4092);
#3273=LINE('',#21251,#4093);
#3274=LINE('',#21253,#4094);
#3275=LINE('',#21263,#4095);
#3276=LINE('',#21269,#4096);
#3277=LINE('',#21275,#4097);
#3278=LINE('',#21281,#4098);
#3279=LINE('',#21287,#4099);
#3280=LINE('',#21304,#4100);
#3281=LINE('',#21306,#4101);
#3282=LINE('',#21308,#4102);
#3283=LINE('',#21310,#4103);
#3284=LINE('',#21312,#4104);
#3285=LINE('',#21314,#4105);
#3286=LINE('',#21316,#4106);
#3287=LINE('',#21321,#4107);
#3288=LINE('',#21323,#4108);
#3289=LINE('',#21325,#4109);
#3290=LINE('',#21329,#4110);
#3291=LINE('',#21331,#4111);
#3292=LINE('',#21333,#4112);
#3293=LINE('',#21334,#4113);
#3294=LINE('',#21336,#4114);
#3295=LINE('',#21340,#4115);
#3296=LINE('',#21344,#4116);
#3297=LINE('',#21348,#4117);
#3298=LINE('',#21352,#4118);
#3299=LINE('',#21354,#4119);
#3300=LINE('',#21356,#4120);
#3301=LINE('',#21360,#4121);
#3302=LINE('',#21364,#4122);
#3303=LINE('',#21368,#4123);
#3304=LINE('',#21373,#4124);
#3305=LINE('',#21375,#4125);
#3306=LINE('',#21377,#4126);
#3307=LINE('',#21381,#4127);
#3308=LINE('',#21385,#4128);
#3309=LINE('',#21389,#4129);
#3310=LINE('',#21391,#4130);
#3311=LINE('',#21395,#4131);
#3312=LINE('',#21399,#4132);
#3313=LINE('',#21403,#4133);
#3314=LINE('',#21406,#4134);
#3315=LINE('',#21408,#4135);
#3316=LINE('',#21410,#4136);
#3317=LINE('',#21412,#4137);
#3318=LINE('',#21414,#4138);
#3319=LINE('',#21416,#4139);
#3320=LINE('',#21418,#4140);
#3321=LINE('',#21421,#4141);
#3322=LINE('',#21423,#4142);
#3323=LINE('',#21427,#4143);
#3324=LINE('',#21428,#4144);
#3325=LINE('',#21430,#4145);
#3326=LINE('',#21432,#4146);
#3327=LINE('',#21434,#4147);
#3328=LINE('',#21436,#4148);
#3329=LINE('',#21438,#4149);
#3330=LINE('',#21440,#4150);
#3331=LINE('',#21442,#4151);
#3332=LINE('',#21446,#4152);
#3333=LINE('',#21447,#4153);
#3334=LINE('',#21449,#4154);
#3335=LINE('',#21451,#4155);
#3336=LINE('',#21454,#4156);
#3337=LINE('',#21455,#4157);
#3338=LINE('',#21457,#4158);
#3339=LINE('',#21459,#4159);
#3340=LINE('',#21461,#4160);
#3341=LINE('',#21462,#4161);
#3342=LINE('',#21464,#4162);
#3343=LINE('',#21466,#4163);
#3344=LINE('',#21549,#4164);
#3345=LINE('',#21573,#4165);
#3346=LINE('',#21651,#4166);
#3347=LINE('',#21675,#4167);
#3348=LINE('',#21715,#4168);
#3349=LINE('',#21757,#4169);
#3350=LINE('',#21763,#4170);
#3351=LINE('',#21820,#4171);
#3352=LINE('',#21824,#4172);
#3353=LINE('',#21978,#4173);
#3354=LINE('',#22002,#4174);
#3355=LINE('',#22080,#4175);
#3356=LINE('',#22104,#4176);
#3357=LINE('',#22144,#4177);
#3358=LINE('',#22186,#4178);
#3359=LINE('',#22192,#4179);
#3360=LINE('',#22249,#4180);
#3361=LINE('',#22253,#4181);
#3362=LINE('',#22359,#4182);
#3363=LINE('',#22366,#4183);
#3364=LINE('',#22370,#4184);
#3365=LINE('',#22377,#4185);
#3366=LINE('',#22380,#4186);
#3367=LINE('',#22463,#4187);
#3368=LINE('',#22470,#4188);
#3369=LINE('',#22474,#4189);
#3370=LINE('',#22481,#4190);
#3371=LINE('',#22484,#4191);
#3372=LINE('',#22552,#4192);
#3373=LINE('',#22558,#4193);
#3374=LINE('',#22564,#4194);
#3375=LINE('',#22570,#4195);
#3376=LINE('',#22576,#4196);
#3377=LINE('',#22580,#4197);
#3378=LINE('',#22584,#4198);
#3379=LINE('',#22588,#4199);
#3380=LINE('',#22592,#4200);
#3381=LINE('',#22613,#4201);
#3382=LINE('',#22617,#4202);
#3383=LINE('',#22623,#4203);
#3384=LINE('',#22630,#4204);
#3385=LINE('',#22634,#4205);
#3386=LINE('',#22650,#4206);
#3387=LINE('',#22651,#4207);
#3388=LINE('',#22653,#4208);
#3389=LINE('',#22654,#4209);
#3390=LINE('',#22656,#4210);
#3391=LINE('',#22658,#4211);
#3392=LINE('',#22660,#4212);
#3393=LINE('',#22661,#4213);
#3394=LINE('',#22663,#4214);
#3395=LINE('',#22664,#4215);
#3396=LINE('',#22668,#4216);
#3397=LINE('',#22670,#4217);
#3398=LINE('',#22671,#4218);
#3399=LINE('',#22674,#4219);
#3400=LINE('',#22676,#4220);
#3401=LINE('',#22677,#4221);
#3402=LINE('',#22680,#4222);
#3403=LINE('',#22682,#4223);
#3404=LINE('',#22683,#4224);
#3405=LINE('',#22685,#4225);
#3406=LINE('',#22686,#4226);
#3407=LINE('',#22691,#4227);
#3408=LINE('',#22693,#4228);
#3409=LINE('',#22694,#4229);
#3410=LINE('',#22697,#4230);
#3411=LINE('',#22699,#4231);
#3412=LINE('',#22700,#4232);
#3413=LINE('',#22703,#4233);
#3414=LINE('',#22705,#4234);
#3415=LINE('',#22706,#4235);
#3416=LINE('',#22708,#4236);
#3417=LINE('',#22709,#4237);
#3418=LINE('',#23176,#4238);
#3419=LINE('',#23181,#4239);
#3420=LINE('',#23201,#4240);
#3421=LINE('',#23206,#4241);
#3422=LINE('',#23220,#4242);
#3423=LINE('',#23228,#4243);
#3424=LINE('',#23231,#4244);
#3425=LINE('',#23241,#4245);
#3426=LINE('',#23247,#4246);
#3427=LINE('',#23283,#4247);
#3428=LINE('',#23289,#4248);
#3429=LINE('',#23292,#4249);
#3430=LINE('',#23297,#4250);
#3431=LINE('',#23300,#4251);
#3432=LINE('',#23302,#4252);
#3433=LINE('',#23319,#4253);
#3434=LINE('',#23325,#4254);
#3435=LINE('',#23361,#4255);
#3436=LINE('',#23367,#4256);
#3437=LINE('',#23370,#4257);
#3438=LINE('',#23375,#4258);
#3439=LINE('',#23378,#4259);
#3440=LINE('',#23380,#4260);
#3441=LINE('',#23391,#4261);
#3442=LINE('',#23399,#4262);
#3443=LINE('',#23402,#4263);
#3444=LINE('',#23408,#4264);
#3445=LINE('',#23420,#4265);
#3446=LINE('',#23433,#4266);
#3447=LINE('',#23471,#4267);
#3448=LINE('',#23509,#4268);
#3449=LINE('',#23547,#4269);
#3450=LINE('',#23585,#4270);
#3451=LINE('',#23623,#4271);
#3452=LINE('',#23661,#4272);
#3453=LINE('',#23699,#4273);
#3454=LINE('',#23737,#4274);
#3455=LINE('',#23775,#4275);
#3456=LINE('',#23813,#4276);
#3457=LINE('',#23851,#4277);
#3458=LINE('',#23889,#4278);
#3459=LINE('',#23928,#4279);
#3460=LINE('',#23960,#4280);
#3461=LINE('',#23992,#4281);
#3462=LINE('',#24068,#4282);
#3463=LINE('',#24146,#4283);
#3464=LINE('',#24222,#4284);
#3465=LINE('',#24298,#4285);
#3466=LINE('',#24374,#4286);
#3467=LINE('',#24450,#4287);
#3468=LINE('',#24526,#4288);
#3469=LINE('',#24604,#4289);
#3470=LINE('',#24680,#4290);
#3471=LINE('',#24756,#4291);
#3472=LINE('',#24857,#4292);
#3473=LINE('',#24869,#4293);
#3474=LINE('',#24875,#4294);
#3475=LINE('',#24892,#4295);
#3476=LINE('',#24938,#4296);
#3477=LINE('',#24939,#4297);
#3478=LINE('',#24940,#4298);
#3479=LINE('',#24943,#4299);
#3480=LINE('',#24944,#4300);
#3481=LINE('',#24948,#4301);
#3482=LINE('',#24950,#4302);
#3483=LINE('',#24952,#4303);
#3484=LINE('',#24957,#4304);
#3485=LINE('',#24959,#4305);
#3486=LINE('',#24961,#4306);
#3487=LINE('',#24965,#4307);
#3488=LINE('',#24966,#4308);
#3489=LINE('',#24970,#4309);
#3490=LINE('',#24972,#4310);
#3491=LINE('',#24974,#4311);
#3492=LINE('',#24979,#4312);
#3493=LINE('',#24981,#4313);
#3494=LINE('',#24983,#4314);
#3495=LINE('',#24988,#4315);
#3496=LINE('',#24990,#4316);
#3497=LINE('',#24992,#4317);
#3498=LINE('',#24993,#4318);
#3499=LINE('',#24996,#4319);
#3500=LINE('',#25000,#4320);
#3501=LINE('',#25004,#4321);
#3502=LINE('',#25006,#4322);
#3503=LINE('',#25011,#4323);
#3504=LINE('',#25014,#4324);
#3505=LINE('',#25018,#4325);
#3506=LINE('',#25019,#4326);
#3507=LINE('',#25029,#4327);
#3508=LINE('',#25030,#4328);
#3509=LINE('',#25957,#4329);
#3510=LINE('',#25996,#4330);
#3511=LINE('',#26034,#4331);
#3512=LINE('',#26072,#4332);
#3513=LINE('',#26110,#4333);
#3514=LINE('',#26148,#4334);
#3515=LINE('',#26186,#4335);
#3516=LINE('',#26224,#4336);
#3517=LINE('',#26236,#4337);
#3518=LINE('',#26249,#4338);
#3519=LINE('',#26270,#4339);
#3520=LINE('',#26293,#4340);
#3521=LINE('',#26334,#4341);
#3522=LINE('',#26412,#4342);
#3523=LINE('',#26488,#4343);
#3524=LINE('',#26564,#4344);
#3525=LINE('',#26640,#4345);
#3526=LINE('',#26716,#4346);
#3527=LINE('',#26792,#4347);
#3528=LINE('',#26905,#4348);
#3529=LINE('',#26910,#4349);
#3530=LINE('',#26912,#4350);
#3531=LINE('',#26914,#4351);
#3532=LINE('',#26916,#4352);
#3533=LINE('',#26918,#4353);
#3534=LINE('',#26920,#4354);
#3535=LINE('',#26922,#4355);
#3536=LINE('',#26924,#4356);
#3537=LINE('',#26926,#4357);
#3538=LINE('',#26928,#4358);
#3539=LINE('',#26930,#4359);
#3540=LINE('',#26931,#4360);
#3541=LINE('',#26963,#4361);
#3542=LINE('',#26965,#4362);
#3543=LINE('',#26967,#4363);
#3544=LINE('',#26969,#4364);
#3545=LINE('',#26971,#4365);
#3546=LINE('',#26972,#4366);
#3547=LINE('',#26976,#4367);
#3548=LINE('',#26978,#4368);
#3549=LINE('',#26979,#4369);
#3550=LINE('',#26980,#4370);
#3551=LINE('',#26982,#4371);
#3552=LINE('',#26984,#4372);
#3553=LINE('',#26985,#4373);
#3554=LINE('',#26988,#4374);
#3555=LINE('',#26989,#4375);
#3556=LINE('',#26990,#4376);
#3557=LINE('',#26992,#4377);
#3558=LINE('',#26994,#4378);
#3559=LINE('',#26995,#4379);
#3560=LINE('',#26998,#4380);
#3561=LINE('',#26999,#4381);
#3562=LINE('',#27000,#4382);
#3563=LINE('',#27002,#4383);
#3564=LINE('',#27003,#4384);
#3565=LINE('',#27005,#4385);
#3566=LINE('',#27006,#4386);
#3567=LINE('',#27697,#4387);
#3568=LINE('',#27705,#4388);
#3569=LINE('',#27710,#4389);
#3570=LINE('',#27713,#4390);
#3571=LINE('',#27723,#4391);
#3572=LINE('',#27731,#4392);
#3573=LINE('',#27734,#4393);
#3574=VECTOR('',#13740,13.);
#3575=VECTOR('',#13747,12.4000000000001);
#3576=VECTOR('',#13754,13.);
#3577=VECTOR('',#13761,16.);
#3578=VECTOR('',#13768,12.4000000000001);
#3579=VECTOR('',#13775,15.4);
#3580=VECTOR('',#13782,1000.);
#3581=VECTOR('',#13785,1000.);
#3582=VECTOR('',#13894,1000.);
#3583=VECTOR('',#13899,1000.);
#3584=VECTOR('',#13916,6.00000000000001);
#3585=VECTOR('',#13921,13.);
#3586=VECTOR('',#13924,13.);
#3587=VECTOR('',#13927,16.);
#3588=VECTOR('',#13930,1000.);
#3589=VECTOR('',#13933,1000.);
#3590=VECTOR('',#13936,9.50000000000001);
#3591=VECTOR('',#13943,5.99999999999999);
#3592=VECTOR('',#13950,8.00000000000001);
#3593=VECTOR('',#13957,7.99999999999999);
#3594=VECTOR('',#13962,13.);
#3595=VECTOR('',#13965,13.);
#3596=VECTOR('',#13968,16.);
#3597=VECTOR('',#13971,9.50000000000001);
#3598=VECTOR('',#13978,5.99999999999999);
#3599=VECTOR('',#13985,8.00000000000001);
#3600=VECTOR('',#13992,7.99999999999999);
#3601=VECTOR('',#13997,9.50000000000001);
#3602=VECTOR('',#14002,5.);
#3603=VECTOR('',#14007,1000.);
#3604=VECTOR('',#14010,1000.);
#3605=VECTOR('',#14015,5.);
#3606=VECTOR('',#14020,1000.);
#3607=VECTOR('',#14021,1000.);
#3608=VECTOR('',#14022,1000.);
#3609=VECTOR('',#14025,1000.);
#3610=VECTOR('',#14028,1000.);
#3611=VECTOR('',#14029,1000.);
#3612=VECTOR('',#14030,1000.);
#3613=VECTOR('',#14031,1000.);
#3614=VECTOR('',#14034,1000.);
#3615=VECTOR('',#14035,1000.);
#3616=VECTOR('',#14036,1000.);
#3617=VECTOR('',#14037,1000.);
#3618=VECTOR('',#14040,1000.);
#3619=VECTOR('',#14041,1000.);
#3620=VECTOR('',#14042,1000.);
#3621=VECTOR('',#14043,1000.);
#3622=VECTOR('',#14048,1000.);
#3623=VECTOR('',#14049,1000.);
#3624=VECTOR('',#14050,1000.);
#3625=VECTOR('',#14051,1000.);
#3626=VECTOR('',#14054,1000.);
#3627=VECTOR('',#14055,1000.);
#3628=VECTOR('',#14056,1000.);
#3629=VECTOR('',#14059,1000.);
#3630=VECTOR('',#14064,1000.);
#3631=VECTOR('',#14071,1000.);
#3632=VECTOR('',#14076,1000.);
#3633=VECTOR('',#14077,1000.);
#3634=VECTOR('',#14078,1000.);
#3635=VECTOR('',#14081,1000.);
#3636=VECTOR('',#14086,1000.);
#3637=VECTOR('',#14087,1000.);
#3638=VECTOR('',#14088,1000.);
#3639=VECTOR('',#14089,1000.);
#3640=VECTOR('',#14092,1000.);
#3641=VECTOR('',#14093,1000.);
#3642=VECTOR('',#14094,1000.);
#3643=VECTOR('',#14095,1000.);
#3644=VECTOR('',#14096,1000.);
#3645=VECTOR('',#14097,1000.);
#3646=VECTOR('',#14102,1000.);
#3647=VECTOR('',#14107,1000.);
#3648=VECTOR('',#14114,1000.);
#3649=VECTOR('',#14115,1000.);
#3650=VECTOR('',#14116,1000.);
#3651=VECTOR('',#14119,1000.);
#3652=VECTOR('',#14120,1000.);
#3653=VECTOR('',#14121,1000.);
#3654=VECTOR('',#14124,1000.);
#3655=VECTOR('',#14125,1000.);
#3656=VECTOR('',#14130,1000.);
#3657=VECTOR('',#14131,1000.);
#3658=VECTOR('',#14138,1000.);
#3659=VECTOR('',#14143,1000.);
#3660=VECTOR('',#14146,1000.);
#3661=VECTOR('',#14147,1000.);
#3662=VECTOR('',#14148,1000.);
#3663=VECTOR('',#14149,1000.);
#3664=VECTOR('',#14152,1000.);
#3665=VECTOR('',#14155,1000.);
#3666=VECTOR('',#14158,1000.);
#3667=VECTOR('',#14163,1000.);
#3668=VECTOR('',#14166,1000.);
#3669=VECTOR('',#14171,1000.);
#3670=VECTOR('',#14174,1000.);
#3671=VECTOR('',#14177,1000.);
#3672=VECTOR('',#14184,1000.);
#3673=VECTOR('',#14187,1000.);
#3674=VECTOR('',#14192,1000.);
#3675=VECTOR('',#14193,1000.);
#3676=VECTOR('',#14194,1000.);
#3677=VECTOR('',#14197,1000.);
#3678=VECTOR('',#14198,1000.);
#3679=VECTOR('',#14199,1000.);
#3680=VECTOR('',#14200,1000.);
#3681=VECTOR('',#14205,1000.);
#3682=VECTOR('',#14212,1000.);
#3683=VECTOR('',#14215,1000.);
#3684=VECTOR('',#14218,1000.);
#3685=VECTOR('',#14221,1000.);
#3686=VECTOR('',#14224,1000.);
#3687=VECTOR('',#14225,1000.);
#3688=VECTOR('',#14230,1000.);
#3689=VECTOR('',#14233,1000.);
#3690=VECTOR('',#14236,1000.);
#3691=VECTOR('',#14239,1000.);
#3692=VECTOR('',#14240,1000.);
#3693=VECTOR('',#14243,1000.);
#3694=VECTOR('',#14244,1000.);
#3695=VECTOR('',#14247,1000.);
#3696=VECTOR('',#14248,1000.);
#3697=VECTOR('',#14251,1000.);
#3698=VECTOR('',#14252,1000.);
#3699=VECTOR('',#14255,1000.);
#3700=VECTOR('',#14256,1000.);
#3701=VECTOR('',#14261,1000.);
#3702=VECTOR('',#14262,1000.);
#3703=VECTOR('',#14265,1000.);
#3704=VECTOR('',#14268,1000.);
#3705=VECTOR('',#14275,1000.);
#3706=VECTOR('',#14276,1000.);
#3707=VECTOR('',#14279,1000.);
#3708=VECTOR('',#14286,1000.);
#3709=VECTOR('',#14287,1000.);
#3710=VECTOR('',#14290,1000.);
#3711=VECTOR('',#14291,1000.);
#3712=VECTOR('',#14292,1000.);
#3713=VECTOR('',#14295,1000.);
#3714=VECTOR('',#14300,1000.);
#3715=VECTOR('',#14303,1000.);
#3716=VECTOR('',#14306,1000.);
#3717=VECTOR('',#14309,1000.);
#3718=VECTOR('',#14310,1000.);
#3719=VECTOR('',#14315,1000.);
#3720=VECTOR('',#14316,1000.);
#3721=VECTOR('',#14317,1000.);
#3722=VECTOR('',#14322,1000.);
#3723=VECTOR('',#14327,1000.);
#3724=VECTOR('',#14328,1000.);
#3725=VECTOR('',#14331,1000.);
#3726=VECTOR('',#14332,1000.);
#3727=VECTOR('',#14333,1000.);
#3728=VECTOR('',#14334,1000.);
#3729=VECTOR('',#14337,1000.);
#3730=VECTOR('',#14352,1000.);
#3731=VECTOR('',#14353,1000.);
#3732=VECTOR('',#14354,1000.);
#3733=VECTOR('',#14355,1000.);
#3734=VECTOR('',#14358,1000.);
#3735=VECTOR('',#14359,1000.);
#3736=VECTOR('',#14360,1000.);
#3737=VECTOR('',#14367,1000.);
#3738=VECTOR('',#14370,1000.);
#3739=VECTOR('',#14373,1000.);
#3740=VECTOR('',#14374,1000.);
#3741=VECTOR('',#14377,1000.);
#3742=VECTOR('',#14380,1000.);
#3743=VECTOR('',#14381,1000.);
#3744=VECTOR('',#14388,1000.);
#3745=VECTOR('',#14389,1000.);
#3746=VECTOR('',#14402,1000.);
#3747=VECTOR('',#14403,1000.);
#3748=VECTOR('',#14404,1000.);
#3749=VECTOR('',#14407,1000.);
#3750=VECTOR('',#14408,1000.);
#3751=VECTOR('',#14411,1000.);
#3752=VECTOR('',#14412,1000.);
#3753=VECTOR('',#14415,1000.);
#3754=VECTOR('',#14416,1000.);
#3755=VECTOR('',#14417,1000.);
#3756=VECTOR('',#14422,1000.);
#3757=VECTOR('',#14431,1000.);
#3758=VECTOR('',#14440,1000.);
#3759=VECTOR('',#14441,1000.);
#3760=VECTOR('',#14444,1000.);
#3761=VECTOR('',#14445,1000.);
#3762=VECTOR('',#14446,1000.);
#3763=VECTOR('',#14453,1000.);
#3764=VECTOR('',#14454,1000.);
#3765=VECTOR('',#14459,1000.);
#3766=VECTOR('',#14462,1000.);
#3767=VECTOR('',#14463,1000.);
#3768=VECTOR('',#14476,1000.);
#3769=VECTOR('',#14477,1000.);
#3770=VECTOR('',#14478,1000.);
#3771=VECTOR('',#14481,1000.);
#3772=VECTOR('',#14482,1000.);
#3773=VECTOR('',#14489,1000.);
#3774=VECTOR('',#14490,1000.);
#3775=VECTOR('',#14491,1000.);
#3776=VECTOR('',#14494,1000.);
#3777=VECTOR('',#14495,1000.);
#3778=VECTOR('',#14500,1000.);
#3779=VECTOR('',#14519,1000.);
#3780=VECTOR('',#14520,1000.);
#3781=VECTOR('',#14521,1000.);
#3782=VECTOR('',#14522,1000.);
#3783=VECTOR('',#14529,1000.);
#3784=VECTOR('',#14530,1000.);
#3785=VECTOR('',#14531,1000.);
#3786=VECTOR('',#14532,1000.);
#3787=VECTOR('',#14537,1000.);
#3788=VECTOR('',#14542,1000.);
#3789=VECTOR('',#14547,1000.);
#3790=VECTOR('',#14552,1000.);
#3791=VECTOR('',#14665,22.5);
#3792=VECTOR('',#14668,22.5);
#3793=VECTOR('',#14671,10.);
#3794=VECTOR('',#14674,10.);
#3795=VECTOR('',#14675,1000.);
#3796=VECTOR('',#14678,1000.);
#3797=VECTOR('',#14679,1000.);
#3798=VECTOR('',#14682,1000.);
#3799=VECTOR('',#14685,1000.);
#3800=VECTOR('',#14694,10.);
#3801=VECTOR('',#14695,10.);
#3802=VECTOR('',#14700,22.5);
#3803=VECTOR('',#14703,22.5);
#3804=VECTOR('',#14706,10.);
#3805=VECTOR('',#14709,10.);
#3806=VECTOR('',#14710,1000.);
#3807=VECTOR('',#14713,1000.);
#3808=VECTOR('',#14714,1000.);
#3809=VECTOR('',#14717,1000.);
#3810=VECTOR('',#14718,1000.);
#3811=VECTOR('',#14719,1000.);
#3812=VECTOR('',#14722,1000.);
#3813=VECTOR('',#14733,10.);
#3814=VECTOR('',#14734,10.);
#3815=VECTOR('',#14739,10.);
#3816=VECTOR('',#14742,10.);
#3817=VECTOR('',#14743,10.);
#3818=VECTOR('',#14748,10.);
#3819=VECTOR('',#14751,10.);
#3820=VECTOR('',#14752,10.);
#3821=VECTOR('',#14755,1000.);
#3822=VECTOR('',#14756,1000.);
#3823=VECTOR('',#14761,1000.);
#3824=VECTOR('',#14764,1000.);
#3825=VECTOR('',#14767,1000.);
#3826=VECTOR('',#14768,1000.);
#3827=VECTOR('',#14777,1000.);
#3828=VECTOR('',#14778,1000.);
#3829=VECTOR('',#14783,14.7);
#3830=VECTOR('',#14792,15.);
#3831=VECTOR('',#14809,11.);
#3832=VECTOR('',#14812,7.99999999999999);
#3833=VECTOR('',#14817,7.99999999999999);
#3834=VECTOR('',#14820,15.);
#3835=VECTOR('',#14823,1000.);
#3836=VECTOR('',#14828,11.);
#3837=VECTOR('',#14833,7.99999999999999);
#3838=VECTOR('',#14838,7.99999999999999);
#3839=VECTOR('',#14843,15.);
#3840=VECTOR('',#14844,1000.);
#3841=VECTOR('',#14847,1000.);
#3842=VECTOR('',#14848,1000.);
#3843=VECTOR('',#14849,1000.);
#3844=VECTOR('',#14850,1000.);
#3845=VECTOR('',#14853,1000.);
#3846=VECTOR('',#14854,1000.);
#3847=VECTOR('',#14855,1000.);
#3848=VECTOR('',#14858,1000.);
#3849=VECTOR('',#14861,1000.);
#3850=VECTOR('',#14862,1000.);
#3851=VECTOR('',#14865,1000.);
#3852=VECTOR('',#14866,1000.);
#3853=VECTOR('',#14869,1000.);
#3854=VECTOR('',#14872,1000.);
#3855=VECTOR('',#14873,1000.);
#3856=VECTOR('',#14876,1000.);
#3857=VECTOR('',#14877,1000.);
#3858=VECTOR('',#14880,1000.);
#3859=VECTOR('',#14883,1000.);
#3860=VECTOR('',#14884,1000.);
#3861=VECTOR('',#14887,1000.);
#3862=VECTOR('',#14894,1000.);
#3863=VECTOR('',#14895,1000.);
#3864=VECTOR('',#14896,1000.);
#3865=VECTOR('',#14931,7.39999999999998);
#3866=VECTOR('',#14938,12.5);
#3867=VECTOR('',#14947,13.);
#3868=VECTOR('',#14954,7.89999999999999);
#3869=VECTOR('',#14957,13.);
#3870=VECTOR('',#14968,7.39999999999998);
#3871=VECTOR('',#14975,12.5);
#3872=VECTOR('',#14982,13.);
#3873=VECTOR('',#14991,7.89999999999999);
#3874=VECTOR('',#14994,13.);
#3875=VECTOR('',#15015,10.5);
#3876=VECTOR('',#15094,12.5);
#3877=VECTOR('',#15115,1000.);
#3878=VECTOR('',#15118,1000.);
#3879=VECTOR('',#15121,1000.);
#3880=VECTOR('',#15124,1000.);
#3881=VECTOR('',#15127,1000.);
#3882=VECTOR('',#15128,1000.);
#3883=VECTOR('',#15131,1000.);
#3884=VECTOR('',#15132,1000.);
#3885=VECTOR('',#15139,1000.);
#3886=VECTOR('',#15140,1000.);
#3887=VECTOR('',#15143,1000.);
#3888=VECTOR('',#15146,1000.);
#3889=VECTOR('',#15149,1000.);
#3890=VECTOR('',#15150,1000.);
#3891=VECTOR('',#15153,1000.);
#3892=VECTOR('',#15154,1000.);
#3893=VECTOR('',#15179,13.5);
#3894=VECTOR('',#15204,13.);
#3895=VECTOR('',#15209,12.5);
#3896=VECTOR('',#15216,18.);
#3897=VECTOR('',#15225,13.5);
#3898=VECTOR('',#15232,13.5);
#3899=VECTOR('',#15237,8.00000000000002);
#3900=VECTOR('',#15244,8.00000000000002);
#3901=VECTOR('',#15251,1000.);
#3902=VECTOR('',#15254,1000.);
#3903=VECTOR('',#15259,8.00000000000002);
#3904=VECTOR('',#15266,1000.);
#3905=VECTOR('',#15269,1000.);
#3906=VECTOR('',#15272,1000.);
#3907=VECTOR('',#15275,1000.);
#3908=VECTOR('',#15278,1000.);
#3909=VECTOR('',#15281,1000.);
#3910=VECTOR('',#15282,1000.);
#3911=VECTOR('',#15287,1000.);
#3912=VECTOR('',#15290,1000.);
#3913=VECTOR('',#15293,1000.);
#3914=VECTOR('',#15294,1000.);
#3915=VECTOR('',#15295,1000.);
#3916=VECTOR('',#15298,1000.);
#3917=VECTOR('',#15299,1000.);
#3918=VECTOR('',#15300,1000.);
#3919=VECTOR('',#15303,1000.);
#3920=VECTOR('',#15306,1000.);
#3921=VECTOR('',#15307,1000.);
#3922=VECTOR('',#15308,1000.);
#3923=VECTOR('',#15311,1000.);
#3924=VECTOR('',#15314,1000.);
#3925=VECTOR('',#15319,1000.);
#3926=VECTOR('',#15320,1000.);
#3927=VECTOR('',#15323,1000.);
#3928=VECTOR('',#15324,1000.);
#3929=VECTOR('',#15325,1000.);
#3930=VECTOR('',#15326,1000.);
#3931=VECTOR('',#15329,1000.);
#3932=VECTOR('',#15330,1000.);
#3933=VECTOR('',#15335,1000.);
#3934=VECTOR('',#15336,1000.);
#3935=VECTOR('',#15337,1000.);
#3936=VECTOR('',#15338,1000.);
#3937=VECTOR('',#15339,1000.);
#3938=VECTOR('',#15340,1000.);
#3939=VECTOR('',#15343,1000.);
#3940=VECTOR('',#15344,1000.);
#3941=VECTOR('',#15347,1000.);
#3942=VECTOR('',#15348,1000.);
#3943=VECTOR('',#15351,1000.);
#3944=VECTOR('',#15352,1000.);
#3945=VECTOR('',#15357,1000.);
#3946=VECTOR('',#15358,1000.);
#3947=VECTOR('',#15359,1000.);
#3948=VECTOR('',#15360,1000.);
#3949=VECTOR('',#15361,1000.);
#3950=VECTOR('',#15362,1000.);
#3951=VECTOR('',#15363,1000.);
#3952=VECTOR('',#15370,1000.);
#3953=VECTOR('',#15371,1000.);
#3954=VECTOR('',#15386,1000.);
#3955=VECTOR('',#15387,1000.);
#3956=VECTOR('',#15412,7.);
#3957=VECTOR('',#15421,8.00000000000001);
#3958=VECTOR('',#15426,8.00000000000001);
#3959=VECTOR('',#15435,7.);
#3960=VECTOR('',#15444,8.);
#3961=VECTOR('',#15449,8.);
#3962=VECTOR('',#15466,8.00000000000002);
#3963=VECTOR('',#15473,8.00000000000001);
#3964=VECTOR('',#15478,1000.);
#3965=VECTOR('',#15481,1000.);
#3966=VECTOR('',#15484,1000.);
#3967=VECTOR('',#15487,1000.);
#3968=VECTOR('',#15492,1000.);
#3969=VECTOR('',#15495,1000.);
#3970=VECTOR('',#15498,1000.);
#3971=VECTOR('',#15501,1000.);
#3972=VECTOR('',#15506,1000.);
#3973=VECTOR('',#15507,1000.);
#3974=VECTOR('',#15510,1000.);
#3975=VECTOR('',#15511,1000.);
#3976=VECTOR('',#15514,1000.);
#3977=VECTOR('',#15515,1000.);
#3978=VECTOR('',#15518,1000.);
#3979=VECTOR('',#15519,1000.);
#3980=VECTOR('',#15534,0.5);
#3981=VECTOR('',#15561,7.50000000000001);
#3982=VECTOR('',#15568,5.00000000000001);
#3983=VECTOR('',#15575,4.25);
#3984=VECTOR('',#15582,8.00000000000001);
#3985=VECTOR('',#15591,1000.);
#3986=VECTOR('',#15596,1000.);
#3987=VECTOR('',#15605,1000.);
#3988=VECTOR('',#15612,1000.);
#3989=VECTOR('',#15617,7.50000000000001);
#3990=VECTOR('',#15634,1000.);
#3991=VECTOR('',#15637,1000.);
#3992=VECTOR('',#15642,23.);
#3993=VECTOR('',#15649,23.5);
#3994=VECTOR('',#15656,25.);
#3995=VECTOR('',#15663,27.);
#3996=VECTOR('',#15674,27.);
#3997=VECTOR('',#15687,13.5);
#3998=VECTOR('',#15688,1000.);
#3999=VECTOR('',#15689,13.5);
#4000=VECTOR('',#15690,1000.);
#4001=VECTOR('',#15693,1000.);
#4002=VECTOR('',#15694,1000.);
#4003=VECTOR('',#15695,1000.);
#4004=VECTOR('',#15696,1000.);
#4005=VECTOR('',#15699,1000.);
#4006=VECTOR('',#15702,1000.);
#4007=VECTOR('',#15703,1000.);
#4008=VECTOR('',#15704,1000.);
#4009=VECTOR('',#15729,1000.);
#4010=VECTOR('',#15730,1000.);
#4011=VECTOR('',#15731,1000.);
#4012=VECTOR('',#15732,1000.);
#4013=VECTOR('',#15733,1000.);
#4014=VECTOR('',#15734,1000.);
#4015=VECTOR('',#15737,1000.);
#4016=VECTOR('',#15738,1000.);
#4017=VECTOR('',#15739,1000.);
#4018=VECTOR('',#15742,1000.);
#4019=VECTOR('',#15743,1000.);
#4020=VECTOR('',#15746,1000.);
#4021=VECTOR('',#15747,1000.);
#4022=VECTOR('',#15750,1000.);
#4023=VECTOR('',#15751,1000.);
#4024=VECTOR('',#15754,1000.);
#4025=VECTOR('',#15755,1000.);
#4026=VECTOR('',#15758,1000.);
#4027=VECTOR('',#15761,1000.);
#4028=VECTOR('',#15762,1000.);
#4029=VECTOR('',#15763,1000.);
#4030=VECTOR('',#15764,1000.);
#4031=VECTOR('',#15765,1000.);
#4032=VECTOR('',#15766,1000.);
#4033=VECTOR('',#15769,1000.);
#4034=VECTOR('',#15770,1000.);
#4035=VECTOR('',#15771,1000.);
#4036=VECTOR('',#15772,10.);
#4037=VECTOR('',#15773,10.);
#4038=VECTOR('',#15774,10.);
#4039=VECTOR('',#15775,10.);
#4040=VECTOR('',#15778,1000.);
#4041=VECTOR('',#15779,1000.);
#4042=VECTOR('',#15780,1000.);
#4043=VECTOR('',#15781,1000.);
#4044=VECTOR('',#15782,1000.);
#4045=VECTOR('',#15785,1000.);
#4046=VECTOR('',#15788,1000.);
#4047=VECTOR('',#15793,1000.);
#4048=VECTOR('',#15796,1000.);
#4049=VECTOR('',#15799,1000.);
#4050=VECTOR('',#15800,1000.);
#4051=VECTOR('',#15803,1000.);
#4052=VECTOR('',#15808,1000.);
#4053=VECTOR('',#15811,1000.);
#4054=VECTOR('',#15812,1000.);
#4055=VECTOR('',#15815,1000.);
#4056=VECTOR('',#15816,1000.);
#4057=VECTOR('',#15819,1000.);
#4058=VECTOR('',#15820,1000.);
#4059=VECTOR('',#15823,1000.);
#4060=VECTOR('',#15824,1000.);
#4061=VECTOR('',#15827,1000.);
#4062=VECTOR('',#15828,1000.);
#4063=VECTOR('',#15831,1000.);
#4064=VECTOR('',#15832,1000.);
#4065=VECTOR('',#15835,1000.);
#4066=VECTOR('',#15838,1000.);
#4067=VECTOR('',#15839,1000.);
#4068=VECTOR('',#15842,1000.);
#4069=VECTOR('',#15843,1000.);
#4070=VECTOR('',#15848,1000.);
#4071=VECTOR('',#15851,1000.);
#4072=VECTOR('',#15856,1000.);
#4073=VECTOR('',#15859,1000.);
#4074=VECTOR('',#15862,1000.);
#4075=VECTOR('',#15865,1000.);
#4076=VECTOR('',#15870,1000.);
#4077=VECTOR('',#15885,1000.);
#4078=VECTOR('',#15888,1000.);
#4079=VECTOR('',#15891,1000.);
#4080=VECTOR('',#15892,1000.);
#4081=VECTOR('',#15895,1000.);
#4082=VECTOR('',#15896,1000.);
#4083=VECTOR('',#15899,1000.);
#4084=VECTOR('',#15902,1000.);
#4085=VECTOR('',#15917,1000.);
#4086=VECTOR('',#15918,1000.);
#4087=VECTOR('',#15921,1000.);
#4088=VECTOR('',#15922,1000.);
#4089=VECTOR('',#15987,14.);
#4090=VECTOR('',#15994,9.00000000000001);
#4091=VECTOR('',#16001,9.00000000000001);
#4092=VECTOR('',#16006,7.50000000000001);
#4093=VECTOR('',#16017,7.50000000000001);
#4094=VECTOR('',#16020,14.);
#4095=VECTOR('',#16035,3.99999999999999);
#4096=VECTOR('',#16042,2.99999999999999);
#4097=VECTOR('',#16049,4.00000000000004);
#4098=VECTOR('',#16056,2.99999999999999);
#4099=VECTOR('',#16063,4.00000000000004);
#4100=VECTOR('',#16090,1000.);
#4101=VECTOR('',#16091,1000.);
#4102=VECTOR('',#16092,1000.);
#4103=VECTOR('',#16093,1000.);
#4104=VECTOR('',#16094,1000.);
#4105=VECTOR('',#16095,1000.);
#4106=VECTOR('',#16096,1000.);
#4107=VECTOR('',#16101,1000.);
#4108=VECTOR('',#16102,1000.);
#4109=VECTOR('',#16103,1000.);
#4110=VECTOR('',#16106,1000.);
#4111=VECTOR('',#16107,1000.);
#4112=VECTOR('',#16108,1000.);
#4113=VECTOR('',#16109,1000.);
#4114=VECTOR('',#16112,1000.);
#4115=VECTOR('',#16115,1000.);
#4116=VECTOR('',#16118,1000.);
#4117=VECTOR('',#16121,1000.);
#4118=VECTOR('',#16124,1000.);
#4119=VECTOR('',#16125,1000.);
#4120=VECTOR('',#16126,1000.);
#4121=VECTOR('',#16129,1000.);
#4122=VECTOR('',#16132,1000.);
#4123=VECTOR('',#16135,1000.);
#4124=VECTOR('',#16140,1000.);
#4125=VECTOR('',#16141,1000.);
#4126=VECTOR('',#16142,1000.);
#4127=VECTOR('',#16145,1000.);
#4128=VECTOR('',#16148,1000.);
#4129=VECTOR('',#16151,1000.);
#4130=VECTOR('',#16154,1000.);
#4131=VECTOR('',#16157,1000.);
#4132=VECTOR('',#16160,1000.);
#4133=VECTOR('',#16163,1000.);
#4134=VECTOR('',#16168,1000.);
#4135=VECTOR('',#16171,1000.);
#4136=VECTOR('',#16174,1000.);
#4137=VECTOR('',#16177,1000.);
#4138=VECTOR('',#16180,1000.);
#4139=VECTOR('',#16183,1000.);
#4140=VECTOR('',#16186,1000.);
#4141=VECTOR('',#16189,1000.);
#4142=VECTOR('',#16190,1000.);
#4143=VECTOR('',#16193,1000.);
#4144=VECTOR('',#16194,1000.);
#4145=VECTOR('',#16197,1000.);
#4146=VECTOR('',#16200,1000.);
#4147=VECTOR('',#16203,1000.);
#4148=VECTOR('',#16206,1000.);
#4149=VECTOR('',#16209,1000.);
#4150=VECTOR('',#16212,1000.);
#4151=VECTOR('',#16215,1000.);
#4152=VECTOR('',#16218,1000.);
#4153=VECTOR('',#16219,1000.);
#4154=VECTOR('',#16220,1000.);
#4155=VECTOR('',#16221,1000.);
#4156=VECTOR('',#16226,1000.);
#4157=VECTOR('',#16227,1000.);
#4158=VECTOR('',#16230,1000.);
#4159=VECTOR('',#16233,1000.);
#4160=VECTOR('',#16236,1000.);
#4161=VECTOR('',#16237,1000.);
#4162=VECTOR('',#16240,1000.);
#4163=VECTOR('',#16243,1000.);
#4164=VECTOR('',#16254,10.);
#4165=VECTOR('',#16255,10.);
#4166=VECTOR('',#16256,10.);
#4167=VECTOR('',#16257,10.);
#4168=VECTOR('',#16260,1.);
#4169=VECTOR('',#16265,4.);
#4170=VECTOR('',#16274,4.);
#4171=VECTOR('',#16287,6.99999999999999);
#4172=VECTOR('',#16292,5.99999999999997);
#4173=VECTOR('',#16301,10.);
#4174=VECTOR('',#16302,10.);
#4175=VECTOR('',#16303,10.);
#4176=VECTOR('',#16304,10.);
#4177=VECTOR('',#16307,1.);
#4178=VECTOR('',#16312,4.00000000000001);
#4179=VECTOR('',#16321,4.00000000000001);
#4180=VECTOR('',#16334,7.);
#4181=VECTOR('',#16339,5.99999999999998);
#4182=VECTOR('',#16384,0.999999999999997);
#4183=VECTOR('',#16393,0.999999999999983);
#4184=VECTOR('',#16398,0.999999999999997);
#4185=VECTOR('',#16407,1.00000000000002);
#4186=VECTOR('',#16412,1.00000000000002);
#4187=VECTOR('',#16447,1.);
#4188=VECTOR('',#16456,0.999999999999989);
#4189=VECTOR('',#16461,1.);
#4190=VECTOR('',#16470,0.999999999999999);
#4191=VECTOR('',#16475,0.999999999999993);
#4192=VECTOR('',#16498,4.50000000000001);
#4193=VECTOR('',#16505,4.99999999999999);
#4194=VECTOR('',#16512,4.50000000000001);
#4195=VECTOR('',#16519,4.99999999999999);
#4196=VECTOR('',#16526,10.);
#4197=VECTOR('',#16529,1000.);
#4198=VECTOR('',#16532,1000.);
#4199=VECTOR('',#16535,1000.);
#4200=VECTOR('',#16538,1000.);
#4201=VECTOR('',#16545,1000.);
#4202=VECTOR('',#16548,1000.);
#4203=VECTOR('',#16553,12.);
#4204=VECTOR('',#16560,1000.);
#4205=VECTOR('',#16563,1000.);
#4206=VECTOR('',#16566,1000.);
#4207=VECTOR('',#16567,1000.);
#4208=VECTOR('',#16568,1000.);
#4209=VECTOR('',#16569,1000.);
#4210=VECTOR('',#16572,1000.);
#4211=VECTOR('',#16573,1000.);
#4212=VECTOR('',#16574,1000.);
#4213=VECTOR('',#16575,1000.);
#4214=VECTOR('',#16578,1000.);
#4215=VECTOR('',#16579,1000.);
#4216=VECTOR('',#16584,1000.);
#4217=VECTOR('',#16585,1000.);
#4218=VECTOR('',#16586,1000.);
#4219=VECTOR('',#16589,1000.);
#4220=VECTOR('',#16590,1000.);
#4221=VECTOR('',#16591,1000.);
#4222=VECTOR('',#16594,1000.);
#4223=VECTOR('',#16595,1000.);
#4224=VECTOR('',#16596,1000.);
#4225=VECTOR('',#16599,1000.);
#4226=VECTOR('',#16600,1000.);
#4227=VECTOR('',#16607,1000.);
#4228=VECTOR('',#16608,1000.);
#4229=VECTOR('',#16609,1000.);
#4230=VECTOR('',#16612,1000.);
#4231=VECTOR('',#16613,1000.);
#4232=VECTOR('',#16614,1000.);
#4233=VECTOR('',#16617,1000.);
#4234=VECTOR('',#16618,1000.);
#4235=VECTOR('',#16619,1000.);
#4236=VECTOR('',#16622,1000.);
#4237=VECTOR('',#16623,1000.);
#4238=VECTOR('',#16660,12.);
#4239=VECTOR('',#16667,14.);
#4240=VECTOR('',#16694,24.);
#4241=VECTOR('',#16699,14.);
#4242=VECTOR('',#16722,5.49999999999999);
#4243=VECTOR('',#16731,6.);
#4244=VECTOR('',#16736,6.);
#4245=VECTOR('',#16749,20.6);
#4246=VECTOR('',#16756,20.);
#4247=VECTOR('',#16801,5.00000000000002);
#4248=VECTOR('',#16808,7.00000000000002);
#4249=VECTOR('',#16813,20.);
#4250=VECTOR('',#16818,15.);
#4251=VECTOR('',#16823,20.);
#4252=VECTOR('',#16826,25.);
#4253=VECTOR('',#16853,20.6);
#4254=VECTOR('',#16860,20.);
#4255=VECTOR('',#16905,5.00000000000001);
#4256=VECTOR('',#16912,7.);
#4257=VECTOR('',#16917,20.);
#4258=VECTOR('',#16922,15.);
#4259=VECTOR('',#16927,20.);
#4260=VECTOR('',#16930,25.);
#4261=VECTOR('',#16947,4.90000000000001);
#4262=VECTOR('',#16956,4.7);
#4263=VECTOR('',#16961,4.90000000000001);
#4264=VECTOR('',#16968,4.45873412499923);
#4265=VECTOR('',#16969,1000.);
#4266=VECTOR('',#16972,4.45873412499923);
#4267=VECTOR('',#16975,4.45873412499923);
#4268=VECTOR('',#16978,4.45873412499923);
#4269=VECTOR('',#16981,4.45873412499923);
#4270=VECTOR('',#16984,4.45873412499923);
#4271=VECTOR('',#16987,4.45873412499923);
#4272=VECTOR('',#16990,4.45873412499923);
#4273=VECTOR('',#16993,4.45873412499923);
#4274=VECTOR('',#16996,4.45873412499923);
#4275=VECTOR('',#16999,4.45873412499923);
#4276=VECTOR('',#17002,4.45873412499923);
#4277=VECTOR('',#17005,4.45873412499923);
#4278=VECTOR('',#17008,5.00000000000001);
#4279=VECTOR('',#17009,5.00000000000001);
#4280=VECTOR('',#17012,1000.);
#4281=VECTOR('',#17015,5.00000000000001);
#4282=VECTOR('',#17018,5.00000000000001);
#4283=VECTOR('',#17021,5.00000000000001);
#4284=VECTOR('',#17024,5.00000000000001);
#4285=VECTOR('',#17027,5.00000000000001);
#4286=VECTOR('',#17030,5.00000000000001);
#4287=VECTOR('',#17033,5.00000000000001);
#4288=VECTOR('',#17036,5.00000000000001);
#4289=VECTOR('',#17039,5.00000000000001);
#4290=VECTOR('',#17042,5.00000000000001);
#4291=VECTOR('',#17045,5.00000000000001);
#4292=VECTOR('',#17054,9.99999999999999);
#4293=VECTOR('',#17067,5.);
#4294=VECTOR('',#17074,5.);
#4295=VECTOR('',#17079,4.35000000000001);
#4296=VECTOR('',#17086,1000.);
#4297=VECTOR('',#17087,1000.);
#4298=VECTOR('',#17088,1000.);
#4299=VECTOR('',#17091,1000.);
#4300=VECTOR('',#17092,1000.);
#4301=VECTOR('',#17095,1000.);
#4302=VECTOR('',#17096,1000.);
#4303=VECTOR('',#17097,1000.);
#4304=VECTOR('',#17102,1000.);
#4305=VECTOR('',#17103,1000.);
#4306=VECTOR('',#17104,1000.);
#4307=VECTOR('',#17109,1000.);
#4308=VECTOR('',#17110,1000.);
#4309=VECTOR('',#17113,1000.);
#4310=VECTOR('',#17114,1000.);
#4311=VECTOR('',#17115,1000.);
#4312=VECTOR('',#17120,1000.);
#4313=VECTOR('',#17121,1000.);
#4314=VECTOR('',#17122,1000.);
#4315=VECTOR('',#17127,1000.);
#4316=VECTOR('',#17128,1000.);
#4317=VECTOR('',#17129,1000.);
#4318=VECTOR('',#17130,1000.);
#4319=VECTOR('',#17133,1000.);
#4320=VECTOR('',#17138,1000.);
#4321=VECTOR('',#17143,1000.);
#4322=VECTOR('',#17144,1000.);
#4323=VECTOR('',#17153,1000.);
#4324=VECTOR('',#17158,1000.);
#4325=VECTOR('',#17165,1000.);
#4326=VECTOR('',#17166,1000.);
#4327=VECTOR('',#17185,1000.);
#4328=VECTOR('',#17186,1000.);
#4329=VECTOR('',#17199,5.54126587500002);
#4330=VECTOR('',#17204,5.54126587500002);
#4331=VECTOR('',#17207,5.54126587500002);
#4332=VECTOR('',#17210,5.54126587500002);
#4333=VECTOR('',#17213,5.54126587500002);
#4334=VECTOR('',#17216,5.54126587500002);
#4335=VECTOR('',#17219,5.54126587500002);
#4336=VECTOR('',#17222,5.54126587500002);
#4337=VECTOR('',#17223,1000.);
#4338=VECTOR('',#17226,5.);
#4339=VECTOR('',#17227,1000.);
#4340=VECTOR('',#17228,5.);
#4341=VECTOR('',#17233,5.);
#4342=VECTOR('',#17236,5.);
#4343=VECTOR('',#17239,5.);
#4344=VECTOR('',#17242,5.);
#4345=VECTOR('',#17245,5.);
#4346=VECTOR('',#17248,5.);
#4347=VECTOR('',#17251,5.);
#4348=VECTOR('',#17260,9.99999999999999);
#4349=VECTOR('',#17265,1000.);
#4350=VECTOR('',#17266,1000.);
#4351=VECTOR('',#17267,1000.);
#4352=VECTOR('',#17268,1000.);
#4353=VECTOR('',#17269,1000.);
#4354=VECTOR('',#17270,1000.);
#4355=VECTOR('',#17271,1000.);
#4356=VECTOR('',#17272,1000.);
#4357=VECTOR('',#17273,1000.);
#4358=VECTOR('',#17274,1000.);
#4359=VECTOR('',#17275,1000.);
#4360=VECTOR('',#17276,1000.);
#4361=VECTOR('',#17279,1000.);
#4362=VECTOR('',#17280,1000.);
#4363=VECTOR('',#17281,1000.);
#4364=VECTOR('',#17282,1000.);
#4365=VECTOR('',#17283,1000.);
#4366=VECTOR('',#17284,1000.);
#4367=VECTOR('',#17289,1000.);
#4368=VECTOR('',#17290,1000.);
#4369=VECTOR('',#17291,1000.);
#4370=VECTOR('',#17292,1000.);
#4371=VECTOR('',#17295,1000.);
#4372=VECTOR('',#17296,1000.);
#4373=VECTOR('',#17297,1000.);
#4374=VECTOR('',#17300,1000.);
#4375=VECTOR('',#17301,1000.);
#4376=VECTOR('',#17302,1000.);
#4377=VECTOR('',#17305,1000.);
#4378=VECTOR('',#17306,1000.);
#4379=VECTOR('',#17307,1000.);
#4380=VECTOR('',#17310,1000.);
#4381=VECTOR('',#17311,1000.);
#4382=VECTOR('',#17312,1000.);
#4383=VECTOR('',#17315,1000.);
#4384=VECTOR('',#17316,1000.);
#4385=VECTOR('',#17319,1000.);
#4386=VECTOR('',#17320,1000.);
#4387=VECTOR('',#17341,9.70000000000001);
#4388=VECTOR('',#17350,6.);
#4389=VECTOR('',#17357,10.);
#4390=VECTOR('',#17360,6.);
#4391=VECTOR('',#17375,6.49999999999999);
#4392=VECTOR('',#17384,7.50000000000001);
#4393=VECTOR('',#17389,7.50000000000001);
#4394=CIRCLE('',#12301,13.);
#4395=CIRCLE('',#12302,12.4);
#4396=CIRCLE('',#12304,13.);
#4397=CIRCLE('',#12305,12.4000000000001);
#4398=CIRCLE('',#12307,13.);
#4399=CIRCLE('',#12308,12.4);
#4400=CIRCLE('',#12310,16.);
#4401=CIRCLE('',#12311,15.3999999999999);
#4402=CIRCLE('',#12313,13.);
#4403=CIRCLE('',#12314,12.4000000000001);
#4404=CIRCLE('',#12316,16.);
#4405=CIRCLE('',#12317,15.4);
#4406=CIRCLE('',#12319,4.5);
#4407=CIRCLE('',#12320,4.5);
#4408=CIRCLE('',#12322,24.);
#4409=CIRCLE('',#12323,6.00000000000001);
#4410=CIRCLE('',#12324,30.);
#4411=CIRCLE('',#12325,6.00000000000001);
#4412=CIRCLE('',#12327,18.);
#4413=CIRCLE('',#12328,2.);
#4414=CIRCLE('',#12329,16.);
#4415=CIRCLE('',#12331,15.);
#4416=CIRCLE('',#12332,2.);
#4417=CIRCLE('',#12333,13.);
#4418=CIRCLE('',#12335,15.);
#4419=CIRCLE('',#12336,2.);
#4420=CIRCLE('',#12337,13.);
#4421=CIRCLE('',#12339,18.);
#4422=CIRCLE('',#12340,2.);
#4423=CIRCLE('',#12341,16.);
#4424=CIRCLE('',#12343,15.);
#4425=CIRCLE('',#12344,2.);
#4426=CIRCLE('',#12345,13.);
#4427=CIRCLE('',#12346,13.);
#4428=CIRCLE('',#12347,2.);
#4429=CIRCLE('',#12349,15.);
#4430=CIRCLE('',#12350,2.);
#4431=CIRCLE('',#12351,13.);
#4432=CIRCLE('',#12352,13.);
#4433=CIRCLE('',#12353,1.99999999999999);
#4434=CIRCLE('',#12355,11.5);
#4435=CIRCLE('',#12356,2.);
#4436=CIRCLE('',#12357,9.50000000000001);
#4437=CIRCLE('',#12358,9.50000000000001);
#4438=CIRCLE('',#12360,11.5);
#4439=CIRCLE('',#12361,2.);
#4440=CIRCLE('',#12362,9.50000000000001);
#4441=CIRCLE('',#12364,9.50000000000001);
#4442=CIRCLE('',#12365,9.50000000000001);
#4443=CIRCLE('',#12366,2.);
#4444=CIRCLE('',#12367,11.5);
#4445=CIRCLE('',#12369,9.50000000000001);
#4446=CIRCLE('',#12370,9.50000000000001);
#4447=CIRCLE('',#12371,2.);
#4448=CIRCLE('',#12372,11.5);
#4449=CIRCLE('',#12374,4.);
#4450=CIRCLE('',#12375,4.);
#4451=CIRCLE('',#12377,4.);
#4452=CIRCLE('',#12379,23.);
#4453=CIRCLE('',#12380,4.);
#4454=CIRCLE('',#12381,27.);
#4455=CIRCLE('',#12382,4.);
#4456=CIRCLE('',#12384,6.00000000000001);
#4457=CIRCLE('',#12385,6.00000000000001);
#4458=CIRCLE('',#12392,9.50000000000001);
#4459=CIRCLE('',#12394,5.99999999999999);
#4460=CIRCLE('',#12395,5.99999999999999);
#4461=CIRCLE('',#12397,8.00000000000001);
#4462=CIRCLE('',#12398,8.00000000000001);
#4463=CIRCLE('',#12400,7.99999999999999);
#4464=CIRCLE('',#12401,7.99999999999999);
#4465=CIRCLE('',#12406,9.50000000000001);
#4466=CIRCLE('',#12408,5.99999999999999);
#4467=CIRCLE('',#12409,5.99999999999999);
#4468=CIRCLE('',#12411,8.00000000000001);
#4469=CIRCLE('',#12412,8.00000000000001);
#4470=CIRCLE('',#12414,7.99999999999999);
#4471=CIRCLE('',#12415,7.99999999999999);
#4472=CIRCLE('',#12418,5.);
#4473=CIRCLE('',#12419,5.);
#4474=CIRCLE('',#12423,5.);
#4475=CIRCLE('',#12424,5.);
#4476=CIRCLE('',#12426,4.);
#4477=CIRCLE('',#12430,4.);
#4478=CIRCLE('',#12433,4.);
#4479=CIRCLE('',#12436,100.);
#4480=CIRCLE('',#12437,100.);
#4481=CIRCLE('',#12438,100.);
#4482=CIRCLE('',#12439,100.);
#4483=CIRCLE('',#12441,53.);
#4484=CIRCLE('',#12442,53.);
#4485=CIRCLE('',#12446,10.);
#4486=CIRCLE('',#12447,10.);
#4487=CIRCLE('',#12454,2.);
#4488=CIRCLE('',#12458,2.);
#4489=CIRCLE('',#12459,2.);
#4490=CIRCLE('',#12460,15.);
#4491=CIRCLE('',#12461,15.);
#4492=CIRCLE('',#12462,15.);
#4493=CIRCLE('',#12463,15.);
#4494=CIRCLE('',#12464,6.00000000000001);
#4495=CIRCLE('',#12467,2.);
#4496=CIRCLE('',#12468,2.);
#4497=CIRCLE('',#12469,15.);
#4498=CIRCLE('',#12470,15.);
#4499=CIRCLE('',#12471,4.5);
#4500=CIRCLE('',#12472,4.5);
#4501=CIRCLE('',#12473,100.);
#4502=CIRCLE('',#12474,100.);
#4503=CIRCLE('',#12475,15.);
#4504=CIRCLE('',#12476,15.);
#4505=CIRCLE('',#12480,10.);
#4506=CIRCLE('',#12481,10.);
#4507=CIRCLE('',#12483,2.);
#4508=CIRCLE('',#12484,2.);
#4509=CIRCLE('',#12485,15.);
#4510=CIRCLE('',#12486,15.);
#4511=CIRCLE('',#12487,100.);
#4512=CIRCLE('',#12488,4.5);
#4513=CIRCLE('',#12489,15.);
#4514=CIRCLE('',#12490,15.);
#4515=CIRCLE('',#12491,6.00000000000001);
#4516=CIRCLE('',#12499,2.);
#4517=CIRCLE('',#12501,30.);
#4518=CIRCLE('',#12507,24.);
#4519=CIRCLE('',#12514,23.);
#4520=CIRCLE('',#12516,2.);
#4521=CIRCLE('',#12518,27.);
#4522=CIRCLE('',#12524,100.);
#4523=CIRCLE('',#12531,53.);
#4524=CIRCLE('',#12532,53.);
#4525=CIRCLE('',#12536,3.99999999999999);
#4526=CIRCLE('',#12541,53.);
#4527=CIRCLE('',#12542,53.);
#4528=CIRCLE('',#12551,2.);
#4529=CIRCLE('',#12552,2.);
#4530=CIRCLE('',#12553,15.);
#4531=CIRCLE('',#12554,15.);
#4532=CIRCLE('',#12555,4.5);
#4533=CIRCLE('',#12556,15.);
#4534=CIRCLE('',#12557,15.);
#4535=CIRCLE('',#12563,2.);
#4536=CIRCLE('',#12572,3.99999999999999);
#4537=CIRCLE('',#12580,53.);
#4538=CIRCLE('',#12581,53.);
#4539=CIRCLE('',#12586,4.);
#4540=CIRCLE('',#12587,4.);
#4541=CIRCLE('',#12590,4.);
#4542=CIRCLE('',#12593,6.50000000000001);
#4543=CIRCLE('',#12594,2.);
#4544=CIRCLE('',#12595,2.);
#4545=CIRCLE('',#12596,6.50000000000001);
#4546=CIRCLE('',#12598,6.50000000000001);
#4547=CIRCLE('',#12599,6.50000000000001);
#4548=CIRCLE('',#12600,2.);
#4549=CIRCLE('',#12601,2.);
#4550=CIRCLE('',#12611,4.);
#4551=CIRCLE('',#12613,4.);
#4552=CIRCLE('',#12615,3.99999999999998);
#4553=CIRCLE('',#12616,3.99999999999998);
#4554=CIRCLE('',#12618,4.);
#4555=CIRCLE('',#12620,4.);
#4556=CIRCLE('',#12622,4.);
#4557=CIRCLE('',#12624,4.);
#4558=CIRCLE('',#12639,6.00000000000001);
#4559=CIRCLE('',#12641,5.99999999999999);
#4560=CIRCLE('',#12655,22.5);
#4561=CIRCLE('',#12656,22.5);
#4562=CIRCLE('',#12658,55.);
#4563=CIRCLE('',#12659,17.);
#4564=CIRCLE('',#12660,7.99999999999999);
#4565=CIRCLE('',#12661,30.);
#4566=CIRCLE('',#12662,25.);
#4567=CIRCLE('',#12663,7.99999999999999);
#4568=CIRCLE('',#12664,11.);
#4569=CIRCLE('',#12667,22.5);
#4570=CIRCLE('',#12668,22.5);
#4571=CIRCLE('',#12670,55.);
#4572=CIRCLE('',#12671,15.);
#4573=CIRCLE('',#12672,7.99999999999999);
#4574=CIRCLE('',#12673,30.);
#4575=CIRCLE('',#12674,25.);
#4576=CIRCLE('',#12675,11.);
#4577=CIRCLE('',#12676,7.99999999999999);
#4578=CIRCLE('',#12677,7.99999999999999);
#4579=CIRCLE('',#12680,55.);
#4580=CIRCLE('',#12683,55.);
#4581=CIRCLE('',#12687,25.);
#4582=CIRCLE('',#12688,30.);
#4583=CIRCLE('',#12689,7.99999999999999);
#4584=CIRCLE('',#12690,17.);
#4585=CIRCLE('',#12691,11.);
#4586=CIRCLE('',#12692,7.99999999999999);
#4587=CIRCLE('',#12695,15.);
#4588=CIRCLE('',#12696,14.7);
#4589=CIRCLE('',#12698,15.);
#4590=CIRCLE('',#12699,15.);
#4591=CIRCLE('',#12700,14.7);
#4592=CIRCLE('',#12702,15.);
#4593=CIRCLE('',#12703,15.);
#4594=CIRCLE('',#12705,15.);
#4595=CIRCLE('',#12706,15.);
#4596=CIRCLE('',#12710,7.99999999999999);
#4597=CIRCLE('',#12712,15.);
#4598=CIRCLE('',#12714,11.);
#4599=CIRCLE('',#12716,7.99999999999999);
#4600=CIRCLE('',#12718,7.99999999999999);
#4601=CIRCLE('',#12719,7.99999999999999);
#4602=CIRCLE('',#12723,30.);
#4603=CIRCLE('',#12725,7.99999999999999);
#4604=CIRCLE('',#12734,25.);
#4605=CIRCLE('',#12740,2.);
#4606=CIRCLE('',#12741,2.);
#4607=CIRCLE('',#12743,2.);
#4608=CIRCLE('',#12744,2.);
#4609=CIRCLE('',#12751,7.89999999999999);
#4610=CIRCLE('',#12752,7.39999999999998);
#4611=CIRCLE('',#12754,13.);
#4612=CIRCLE('',#12755,12.5);
#4613=CIRCLE('',#12757,13.);
#4614=CIRCLE('',#12758,13.);
#4615=CIRCLE('',#12759,12.5);
#4616=CIRCLE('',#12761,7.89999999999999);
#4617=CIRCLE('',#12767,7.89999999999999);
#4618=CIRCLE('',#12768,7.39999999999998);
#4619=CIRCLE('',#12770,13.);
#4620=CIRCLE('',#12771,12.5);
#4621=CIRCLE('',#12773,13.);
#4622=CIRCLE('',#12774,12.5);
#4623=CIRCLE('',#12775,13.);
#4624=CIRCLE('',#12777,7.89999999999999);
#4625=CIRCLE('',#12787,12.5);
#4626=CIRCLE('',#12788,12.5);
#4627=CIRCLE('',#12789,10.5);
#4628=CIRCLE('',#12791,36.6405776438474);
#4629=CIRCLE('',#12792,37.1705339516543);
#4630=CIRCLE('',#12794,27.867569521218);
#4631=CIRCLE('',#12795,26.7352152856439);
#4632=CIRCLE('',#12796,30.4789811536249);
#4633=CIRCLE('',#12797,26.7352152856439);
#4634=CIRCLE('',#12798,27.867569521218);
#4635=CIRCLE('',#12799,26.7352152856438);
#4636=CIRCLE('',#12800,30.4789811536249);
#4637=CIRCLE('',#12801,26.7352152856439);
#4638=CIRCLE('',#12802,27.867569521218);
#4639=CIRCLE('',#12803,26.7352152856439);
#4640=CIRCLE('',#12804,30.4789811536249);
#4641=CIRCLE('',#12805,26.7352152856439);
#4642=CIRCLE('',#12806,27.867569521218);
#4643=CIRCLE('',#12807,26.7352152856439);
#4644=CIRCLE('',#12808,30.4789811536249);
#4645=CIRCLE('',#12809,26.7352152856439);
#4646=CIRCLE('',#12811,37.1705339516543);
#4647=CIRCLE('',#12812,37.0952876899206);
#4648=CIRCLE('',#12813,37.6405776438474);
#4649=CIRCLE('',#12814,37.0952876899207);
#4650=CIRCLE('',#12815,37.0952876899206);
#4651=CIRCLE('',#12816,37.6405776438474);
#4652=CIRCLE('',#12817,37.0952876899206);
#4653=CIRCLE('',#12818,37.1705339516542);
#4654=CIRCLE('',#12819,37.0952876899206);
#4655=CIRCLE('',#12820,37.6405776438474);
#4656=CIRCLE('',#12821,37.0952876899206);
#4657=CIRCLE('',#12822,37.1705339516543);
#4658=CIRCLE('',#12823,37.0952876899207);
#4659=CIRCLE('',#12824,37.6405776438474);
#4660=CIRCLE('',#12825,37.0952876899206);
#4661=CIRCLE('',#12826,12.5);
#4662=CIRCLE('',#12829,34.6617737272029);
#4663=CIRCLE('',#12831,34.6617737272029);
#4664=CIRCLE('',#12833,34.6617737272029);
#4665=CIRCLE('',#12836,34.6617737272029);
#4666=CIRCLE('',#12838,36.6405776438474);
#4667=CIRCLE('',#12844,36.6405776438474);
#4668=CIRCLE('',#12851,36.6405776438474);
#4669=CIRCLE('',#12861,13.5);
#4670=CIRCLE('',#12862,14.5);
#4671=CIRCLE('',#12864,15.);
#4672=CIRCLE('',#12865,2.);
#4673=CIRCLE('',#12866,13.);
#4674=CIRCLE('',#12867,13.);
#4675=CIRCLE('',#12869,15.);
#4676=CIRCLE('',#12870,2.);
#4677=CIRCLE('',#12871,13.);
#4678=CIRCLE('',#12872,13.);
#4679=CIRCLE('',#12875,12.5);
#4680=CIRCLE('',#12876,12.5);
#4681=CIRCLE('',#12878,18.);
#4682=CIRCLE('',#12879,18.);
#4683=CIRCLE('',#12880,18.);
#4684=CIRCLE('',#12882,13.5);
#4685=CIRCLE('',#12883,13.5);
#4686=CIRCLE('',#12885,13.5);
#4687=CIRCLE('',#12887,8.00000000000002);
#4688=CIRCLE('',#12888,8.00000000000002);
#4689=CIRCLE('',#12890,8.00000000000002);
#4690=CIRCLE('',#12891,8.);
#4691=CIRCLE('',#12893,15.);
#4692=CIRCLE('',#12894,15.);
#4693=CIRCLE('',#12896,7.99999999999999);
#4694=CIRCLE('',#12897,8.00000000000002);
#4695=CIRCLE('',#12899,15.);
#4696=CIRCLE('',#12900,15.);
#4697=CIRCLE('',#12902,3.);
#4698=CIRCLE('',#12903,2.99999999999999);
#4699=CIRCLE('',#12906,2.99999999999999);
#4700=CIRCLE('',#12907,3.);
#4701=CIRCLE('',#12911,20.);
#4702=CIRCLE('',#12912,20.);
#4703=CIRCLE('',#12914,20.);
#4704=CIRCLE('',#12915,20.);
#4705=CIRCLE('',#12918,8.00000000000002);
#4706=CIRCLE('',#12919,8.00000000000002);
#4707=CIRCLE('',#12923,8.00000000000001);
#4708=CIRCLE('',#12924,8.00000000000001);
#4709=CIRCLE('',#12929,20.);
#4710=CIRCLE('',#12930,20.);
#4711=CIRCLE('',#12932,20.);
#4712=CIRCLE('',#12933,20.);
#4713=CIRCLE('',#12946,8.00000000000001);
#4714=CIRCLE('',#12947,7.);
#4715=CIRCLE('',#12949,8.00000000000001);
#4716=CIRCLE('',#12950,8.00000000000001);
#4717=CIRCLE('',#12951,7.);
#4718=CIRCLE('',#12956,8.);
#4719=CIRCLE('',#12957,7.);
#4720=CIRCLE('',#12959,8.);
#4721=CIRCLE('',#12960,8.);
#4722=CIRCLE('',#12961,7.);
#4723=CIRCLE('',#12970,7.99999999999999);
#4724=CIRCLE('',#12971,7.99999999999999);
#4725=CIRCLE('',#12973,8.00000000000001);
#4726=CIRCLE('',#12974,8.00000000000001);
#4727=CIRCLE('',#12976,10.);
#4728=CIRCLE('',#12977,10.);
#4729=CIRCLE('',#12978,10.);
#4730=CIRCLE('',#12979,10.);
#4731=CIRCLE('',#12981,10.);
#4732=CIRCLE('',#12982,10.);
#4733=CIRCLE('',#12983,10.);
#4734=CIRCLE('',#12984,10.);
#4735=CIRCLE('',#12996,0.5);
#4736=CIRCLE('',#12998,11.5);
#4737=CIRCLE('',#12999,2.);
#4738=CIRCLE('',#13000,13.5);
#4739=CIRCLE('',#13001,13.5);
#4740=CIRCLE('',#13003,13.5);
#4741=CIRCLE('',#13004,13.5);
#4742=CIRCLE('',#13005,2.);
#4743=CIRCLE('',#13006,11.5);
#4744=CIRCLE('',#13008,7.50000000000001);
#4745=CIRCLE('',#13009,7.50000000000001);
#4746=CIRCLE('',#13011,5.);
#4747=CIRCLE('',#13012,5.);
#4748=CIRCLE('',#13014,4.25);
#4749=CIRCLE('',#13015,4.25);
#4750=CIRCLE('',#13017,8.00000000000001);
#4751=CIRCLE('',#13018,8.00000000000001);
#4752=CIRCLE('',#13032,7.50000000000001);
#4753=CIRCLE('',#13033,7.50000000000001);
#4754=CIRCLE('',#13034,7.50000000000001);
#4755=CIRCLE('',#13035,7.50000000000001);
#4756=CIRCLE('',#13036,7.50000000000001);
#4757=CIRCLE('',#13037,7.50000000000001);
#4758=CIRCLE('',#13038,7.50000000000001);
#4759=CIRCLE('',#13040,10.);
#4760=CIRCLE('',#13041,9.99999999999999);
#4761=CIRCLE('',#13043,23.);
#4762=CIRCLE('',#13044,23.);
#4763=CIRCLE('',#13046,23.5);
#4764=CIRCLE('',#13047,23.5);
#4765=CIRCLE('',#13049,25.);
#4766=CIRCLE('',#13050,25.);
#4767=CIRCLE('',#13052,27.);
#4768=CIRCLE('',#13053,27.);
#4769=CIRCLE('',#13054,27.);
#4770=CIRCLE('',#13055,27.);
#4771=CIRCLE('',#13058,23.);
#4772=CIRCLE('',#13059,23.);
#4773=CIRCLE('',#13060,23.);
#4774=CIRCLE('',#13061,23.);
#4775=CIRCLE('',#13062,23.);
#4776=CIRCLE('',#13070,2.);
#4777=CIRCLE('',#13071,2.);
#4778=CIRCLE('',#13073,2.);
#4779=CIRCLE('',#13074,2.);
#4780=CIRCLE('',#13092,3.00000000000001);
#4781=CIRCLE('',#13095,2.99999999999999);
#4782=CIRCLE('',#13139,2.);
#4783=CIRCLE('',#13140,2.00000000000002);
#4784=CIRCLE('',#13141,2.00000000000001);
#4785=CIRCLE('',#13143,1.99999999999999);
#4786=CIRCLE('',#13145,2.);
#4787=CIRCLE('',#13147,1.99999999999999);
#4788=CIRCLE('',#13149,1.99999999999999);
#4789=CIRCLE('',#13150,2.00000000000002);
#4790=CIRCLE('',#13166,14.);
#4791=CIRCLE('',#13167,14.);
#4792=CIRCLE('',#13168,12.);
#4793=CIRCLE('',#13169,14.);
#4794=CIRCLE('',#13171,9.00000000000001);
#4795=CIRCLE('',#13173,9.00000000000001);
#4796=CIRCLE('',#13175,14.);
#4797=CIRCLE('',#13176,7.50000000000001);
#4798=CIRCLE('',#13177,7.50000000000001);
#4799=CIRCLE('',#13178,14.);
#4800=CIRCLE('',#13180,7.50000000000001);
#4801=CIRCLE('',#13188,3.99999999999999);
#4802=CIRCLE('',#13189,3.99999999999999);
#4803=CIRCLE('',#13191,2.99999999999999);
#4804=CIRCLE('',#13192,2.99999999999999);
#4805=CIRCLE('',#13194,3.99999999999999);
#4806=CIRCLE('',#13195,4.00000000000003);
#4807=CIRCLE('',#13197,2.99999999999999);
#4808=CIRCLE('',#13198,2.99999999999999);
#4809=CIRCLE('',#13200,4.00000000000003);
#4810=CIRCLE('',#13201,4.00000000000003);
#4811=CIRCLE('',#13210,0.925000000000001);
#4812=CIRCLE('',#13211,3.02500000000001);
#4813=CIRCLE('',#13214,3.37500000000002);
#4814=CIRCLE('',#13216,3.37500000000002);
#4815=CIRCLE('',#13218,3.49999999999998);
#4816=CIRCLE('',#13219,5.50000000000002);
#4817=CIRCLE('',#13220,5.50000000000002);
#4818=CIRCLE('',#13221,3.49999999999998);
#4819=CIRCLE('',#13222,1.99999999999999);
#4820=CIRCLE('',#13223,3.99999999999998);
#4821=CIRCLE('',#13224,3.99999999999998);
#4822=CIRCLE('',#13225,1.99999999999999);
#4823=CIRCLE('',#13227,3.49999999999998);
#4824=CIRCLE('',#13228,5.50000000000002);
#4825=CIRCLE('',#13229,5.50000000000002);
#4826=CIRCLE('',#13230,3.49999999999998);
#4827=CIRCLE('',#13231,1.99999999999999);
#4828=CIRCLE('',#13232,3.99999999999998);
#4829=CIRCLE('',#13233,3.99999999999998);
#4830=CIRCLE('',#13234,1.99999999999999);
#4831=CIRCLE('',#13243,3.37500000000002);
#4832=CIRCLE('',#13252,3.37500000000002);
#4833=CIRCLE('',#13266,4.);
#4834=CIRCLE('',#13267,2.84529946162073);
#4835=CIRCLE('',#13268,4.);
#4836=CIRCLE('',#13270,4.);
#4837=CIRCLE('',#13272,4.59999999999999);
#4838=CIRCLE('',#13273,0.6);
#4839=CIRCLE('',#13275,6.99999999999999);
#4840=CIRCLE('',#13276,6.99999999999999);
#4841=CIRCLE('',#13277,6.99999999999999);
#4842=CIRCLE('',#13279,5.99999999999997);
#4843=CIRCLE('',#13285,4.00000000000001);
#4844=CIRCLE('',#13286,2.84529946162074);
#4845=CIRCLE('',#13287,4.00000000000001);
#4846=CIRCLE('',#13289,4.00000000000001);
#4847=CIRCLE('',#13291,4.6);
#4848=CIRCLE('',#13292,0.6);
#4849=CIRCLE('',#13294,7.);
#4850=CIRCLE('',#13295,7.);
#4851=CIRCLE('',#13296,7.);
#4852=CIRCLE('',#13298,5.99999999999998);
#4853=CIRCLE('',#13304,0.999999999999987);
#4854=CIRCLE('',#13305,4.00000000000001);
#4855=CIRCLE('',#13306,0.999999999999987);
#4856=CIRCLE('',#13308,0.999999999999987);
#4857=CIRCLE('',#13309,4.00000000000001);
#4858=CIRCLE('',#13310,0.999999999999987);
#4859=CIRCLE('',#13312,1.);
#4860=CIRCLE('',#13313,1.);
#4861=CIRCLE('',#13314,1.00000000000001);
#4862=CIRCLE('',#13316,1.00000000000002);
#4863=CIRCLE('',#13317,1.00000000000002);
#4864=CIRCLE('',#13318,0.999999999999996);
#4865=CIRCLE('',#13320,0.999999999999987);
#4866=CIRCLE('',#13321,0.999999999999987);
#4867=CIRCLE('',#13323,0.999999999999987);
#4868=CIRCLE('',#13324,0.999999999999987);
#4869=CIRCLE('',#13326,0.999999999999987);
#4870=CIRCLE('',#13327,0.999999999999987);
#4871=CIRCLE('',#13329,0.999999999999987);
#4872=CIRCLE('',#13330,0.999999999999987);
#4873=CIRCLE('',#13333,1.00000000000001);
#4874=CIRCLE('',#13334,4.);
#4875=CIRCLE('',#13335,1.00000000000001);
#4876=CIRCLE('',#13337,1.00000000000001);
#4877=CIRCLE('',#13338,4.);
#4878=CIRCLE('',#13339,1.00000000000001);
#4879=CIRCLE('',#13341,1.00000000000002);
#4880=CIRCLE('',#13342,1.00000000000002);
#4881=CIRCLE('',#13343,1.00000000000001);
#4882=CIRCLE('',#13345,0.999999999999993);
#4883=CIRCLE('',#13346,1.00000000000001);
#4884=CIRCLE('',#13347,0.999999999999993);
#4885=CIRCLE('',#13349,1.00000000000001);
#4886=CIRCLE('',#13350,1.00000000000001);
#4887=CIRCLE('',#13352,1.00000000000001);
#4888=CIRCLE('',#13353,1.00000000000001);
#4889=CIRCLE('',#13355,1.00000000000001);
#4890=CIRCLE('',#13356,1.00000000000001);
#4891=CIRCLE('',#13358,1.00000000000001);
#4892=CIRCLE('',#13359,1.00000000000001);
#4893=CIRCLE('',#13371,4.50000000000001);
#4894=CIRCLE('',#13372,4.50000000000001);
#4895=CIRCLE('',#13374,4.99999999999999);
#4896=CIRCLE('',#13375,4.99999999999999);
#4897=CIRCLE('',#13377,4.50000000000001);
#4898=CIRCLE('',#13378,4.50000000000001);
#4899=CIRCLE('',#13380,4.99999999999999);
#4900=CIRCLE('',#13381,4.99999999999999);
#4901=CIRCLE('',#13383,10.);
#4902=CIRCLE('',#13384,10.);
#4903=CIRCLE('',#13385,10.);
#4904=CIRCLE('',#13386,10.);
#4905=CIRCLE('',#13387,10.);
#4906=CIRCLE('',#13388,10.);
#4907=CIRCLE('',#13390,12.);
#4908=CIRCLE('',#13391,12.);
#4909=CIRCLE('',#13392,12.);
#4910=CIRCLE('',#13393,12.);
#4911=CIRCLE('',#13394,12.);
#4912=CIRCLE('',#13395,12.);
#4913=CIRCLE('',#13396,12.);
#4914=CIRCLE('',#13397,12.);
#4915=CIRCLE('',#13415,27.);
#4916=CIRCLE('',#13416,27.);
#4917=CIRCLE('',#13418,13.);
#4918=CIRCLE('',#13424,12.);
#4919=CIRCLE('',#13425,12.);
#4920=CIRCLE('',#13426,2.);
#4921=CIRCLE('',#13427,14.);
#4922=CIRCLE('',#13428,14.);
#4923=CIRCLE('',#13430,12.);
#4924=CIRCLE('',#13432,14.);
#4925=CIRCLE('',#13436,22.);
#4926=CIRCLE('',#13437,2.);
#4927=CIRCLE('',#13438,24.);
#4928=CIRCLE('',#13439,24.);
#4929=CIRCLE('',#13441,24.);
#4930=CIRCLE('',#13442,24.);
#4931=CIRCLE('',#13443,2.);
#4932=CIRCLE('',#13444,22.);
#4933=CIRCLE('',#13447,14.);
#4934=CIRCLE('',#13448,14.);
#4935=CIRCLE('',#13458,6.00000000000001);
#4936=CIRCLE('',#13459,5.49999999999999);
#4937=CIRCLE('',#13461,6.);
#4938=CIRCLE('',#13462,6.);
#4939=CIRCLE('',#13463,5.49999999999997);
#4940=CIRCLE('',#13469,20.);
#4941=CIRCLE('',#13470,20.);
#4942=CIRCLE('',#13471,20.6);
#4943=CIRCLE('',#13473,20.);
#4944=CIRCLE('',#13474,20.6);
#4945=CIRCLE('',#13476,23.);
#4946=CIRCLE('',#13477,2.);
#4947=CIRCLE('',#13478,25.);
#4948=CIRCLE('',#13479,25.);
#4949=CIRCLE('',#13481,18.);
#4950=CIRCLE('',#13482,2.);
#4951=CIRCLE('',#13483,20.);
#4952=CIRCLE('',#13485,25.);
#4953=CIRCLE('',#13486,25.);
#4954=CIRCLE('',#13487,2.);
#4955=CIRCLE('',#13488,23.);
#4956=CIRCLE('',#13490,18.);
#4957=CIRCLE('',#13491,2.);
#4958=CIRCLE('',#13492,20.);
#4959=CIRCLE('',#13493,20.);
#4960=CIRCLE('',#13495,4.99999999999998);
#4961=CIRCLE('',#13496,5.00000000000002);
#4962=CIRCLE('',#13498,15.);
#4963=CIRCLE('',#13499,7.00000000000002);
#4964=CIRCLE('',#13502,15.);
#4965=CIRCLE('',#13503,7.00000000000002);
#4966=CIRCLE('',#13517,20.);
#4967=CIRCLE('',#13518,20.);
#4968=CIRCLE('',#13519,20.6);
#4969=CIRCLE('',#13521,20.);
#4970=CIRCLE('',#13522,20.6);
#4971=CIRCLE('',#13524,23.);
#4972=CIRCLE('',#13525,2.);
#4973=CIRCLE('',#13526,25.);
#4974=CIRCLE('',#13527,25.);
#4975=CIRCLE('',#13529,18.);
#4976=CIRCLE('',#13530,2.);
#4977=CIRCLE('',#13531,20.);
#4978=CIRCLE('',#13533,25.);
#4979=CIRCLE('',#13534,25.);
#4980=CIRCLE('',#13535,2.);
#4981=CIRCLE('',#13536,23.);
#4982=CIRCLE('',#13538,18.);
#4983=CIRCLE('',#13539,2.);
#4984=CIRCLE('',#13540,20.);
#4985=CIRCLE('',#13541,20.);
#4986=CIRCLE('',#13543,5.00000000000001);
#4987=CIRCLE('',#13544,5.00000000000001);
#4988=CIRCLE('',#13546,15.);
#4989=CIRCLE('',#13547,7.);
#4990=CIRCLE('',#13550,15.);
#4991=CIRCLE('',#13551,7.);
#4992=CIRCLE('',#13561,4.90000000000001);
#4993=CIRCLE('',#13562,4.70000000000039);
#4994=CIRCLE('',#13564,4.90000000000002);
#4995=CIRCLE('',#13565,4.90000000000002);
#4996=CIRCLE('',#13566,4.70000000000003);
#4997=CIRCLE('',#13584,5.00000000000001);
#4998=CIRCLE('',#13597,5.00000000000001);
#4999=CIRCLE('',#13599,9.99999999999999);
#5000=CIRCLE('',#13600,10.);
#5001=CIRCLE('',#13601,10.);
#5002=CIRCLE('',#13602,10.);
#5003=CIRCLE('',#13603,10.);
#5004=CIRCLE('',#13605,5.);
#5005=CIRCLE('',#13606,5.);
#5006=CIRCLE('',#13608,5.);
#5007=CIRCLE('',#13609,5.);
#5008=CIRCLE('',#13611,4.35000000000001);
#5009=CIRCLE('',#13612,4.45873412500005);
#5010=CIRCLE('',#13616,9.);
#5011=CIRCLE('',#13618,9.);
#5012=CIRCLE('',#13621,9.);
#5013=CIRCLE('',#13623,9.);
#5014=CIRCLE('',#13626,4.99999999999998);
#5015=CIRCLE('',#13627,4.99999999999998);
#5016=CIRCLE('',#13629,4.99999999999998);
#5017=CIRCLE('',#13630,4.99999999999998);
#5018=CIRCLE('',#13654,5.5412658750012);
#5019=CIRCLE('',#13663,5.);
#5020=CIRCLE('',#13671,5.);
#5021=CIRCLE('',#13674,9.99999999999999);
#5022=CIRCLE('',#13675,9.99999999999999);
#5023=CIRCLE('',#13695,10.);
#5024=CIRCLE('',#13696,9.7);
#5025=CIRCLE('',#13698,6.);
#5026=CIRCLE('',#13699,6.);
#5027=CIRCLE('',#13700,5.4);
#5028=CIRCLE('',#13702,10.);
#5029=CIRCLE('',#13704,6.);
#5030=CIRCLE('',#13710,7.50000000000001);
#5031=CIRCLE('',#13711,6.49999999999999);
#5032=CIRCLE('',#13713,7.50000000000001);
#5033=CIRCLE('',#13714,7.50000000000001);
#5034=CIRCLE('',#13715,6.50000000000003);
#5035=VERTEX_POINT('',#17423);
#5036=VERTEX_POINT('',#17425);
#5037=VERTEX_POINT('',#17429);
#5038=VERTEX_POINT('',#17431);
#5039=VERTEX_POINT('',#17435);
#5040=VERTEX_POINT('',#17437);
#5041=VERTEX_POINT('',#17441);
#5042=VERTEX_POINT('',#17443);
#5043=VERTEX_POINT('',#17447);
#5044=VERTEX_POINT('',#17449);
#5045=VERTEX_POINT('',#17453);
#5046=VERTEX_POINT('',#17455);
#5047=VERTEX_POINT('',#17459);
#5048=VERTEX_POINT('',#17460);
#5049=VERTEX_POINT('',#17462);
#5050=VERTEX_POINT('',#17464);
#5051=VERTEX_POINT('',#17466);
#5052=VERTEX_POINT('',#17481);
#5053=VERTEX_POINT('',#17482);
#5054=VERTEX_POINT('',#17484);
#5055=VERTEX_POINT('',#17486);
#5056=VERTEX_POINT('',#17490);
#5057=VERTEX_POINT('',#17492);
#5058=VERTEX_POINT('',#17496);
#5059=VERTEX_POINT('',#17498);
#5060=VERTEX_POINT('',#17502);
#5061=VERTEX_POINT('',#17504);
#5062=VERTEX_POINT('',#17508);
#5063=VERTEX_POINT('',#17510);
#5064=VERTEX_POINT('',#17514);
#5065=VERTEX_POINT('',#17515);
#5066=VERTEX_POINT('',#17517);
#5067=VERTEX_POINT('',#17519);
#5068=VERTEX_POINT('',#17521);
#5069=VERTEX_POINT('',#17525);
#5070=VERTEX_POINT('',#17526);
#5071=VERTEX_POINT('',#17528);
#5072=VERTEX_POINT('',#17530);
#5073=VERTEX_POINT('',#17532);
#5074=VERTEX_POINT('',#17536);
#5075=VERTEX_POINT('',#17538);
#5076=VERTEX_POINT('',#17540);
#5077=VERTEX_POINT('',#17544);
#5078=VERTEX_POINT('',#17546);
#5079=VERTEX_POINT('',#17550);
#5080=VERTEX_POINT('',#17551);
#5081=VERTEX_POINT('',#17554);
#5082=VERTEX_POINT('',#17558);
#5083=VERTEX_POINT('',#17559);
#5084=VERTEX_POINT('',#17562);
#5085=VERTEX_POINT('',#17566);
#5086=VERTEX_POINT('',#17567);
#5087=VERTEX_POINT('',#17569);
#5088=VERTEX_POINT('',#17571);
#5089=VERTEX_POINT('',#17573);
#5090=VERTEX_POINT('',#17575);
#5091=VERTEX_POINT('',#17579);
#5092=VERTEX_POINT('',#17580);
#5093=VERTEX_POINT('',#17582);
#5094=VERTEX_POINT('',#17584);
#5095=VERTEX_POINT('',#17588);
#5096=VERTEX_POINT('',#17590);
#5097=VERTEX_POINT('',#17612);
#5098=VERTEX_POINT('',#17614);
#5099=VERTEX_POINT('',#17618);
#5100=VERTEX_POINT('',#17622);
#5101=VERTEX_POINT('',#17624);
#5102=VERTEX_POINT('',#17628);
#5103=VERTEX_POINT('',#17630);
#5104=VERTEX_POINT('',#17634);
#5105=VERTEX_POINT('',#17636);
#5106=VERTEX_POINT('',#17658);
#5107=VERTEX_POINT('',#17662);
#5108=VERTEX_POINT('',#17664);
#5109=VERTEX_POINT('',#17668);
#5110=VERTEX_POINT('',#17670);
#5111=VERTEX_POINT('',#17674);
#5112=VERTEX_POINT('',#17676);
#5113=VERTEX_POINT('',#17682);
#5114=VERTEX_POINT('',#17684);
#5115=VERTEX_POINT('',#17688);
#5116=VERTEX_POINT('',#17690);
#5117=VERTEX_POINT('',#17694);
#5118=VERTEX_POINT('',#17696);
#5119=VERTEX_POINT('',#17700);
#5120=VERTEX_POINT('',#17701);
#5121=VERTEX_POINT('',#17703);
#5122=VERTEX_POINT('',#17705);
#5123=VERTEX_POINT('',#17707);
#5124=VERTEX_POINT('',#17711);
#5125=VERTEX_POINT('',#17712);
#5126=VERTEX_POINT('',#17714);
#5127=VERTEX_POINT('',#17716);
#5128=VERTEX_POINT('',#17720);
#5129=VERTEX_POINT('',#17722);
#5130=VERTEX_POINT('',#17724);
#5131=VERTEX_POINT('',#17728);
#5132=VERTEX_POINT('',#17729);
#5133=VERTEX_POINT('',#17731);
#5134=VERTEX_POINT('',#17733);
#5135=VERTEX_POINT('',#17735);
#5136=VERTEX_POINT('',#17739);
#5137=VERTEX_POINT('',#17740);
#5138=VERTEX_POINT('',#17742);
#5139=VERTEX_POINT('',#17744);
#5140=VERTEX_POINT('',#17748);
#5141=VERTEX_POINT('',#17749);
#5142=VERTEX_POINT('',#17751);
#5143=VERTEX_POINT('',#17753);
#5144=VERTEX_POINT('',#17755);
#5145=VERTEX_POINT('',#17759);
#5146=VERTEX_POINT('',#17760);
#5147=VERTEX_POINT('',#17762);
#5148=VERTEX_POINT('',#17766);
#5149=VERTEX_POINT('',#17768);
#5150=VERTEX_POINT('',#17770);
#5151=VERTEX_POINT('',#17779);
#5152=VERTEX_POINT('',#17780);
#5153=VERTEX_POINT('',#17782);
#5154=VERTEX_POINT('',#17784);
#5155=VERTEX_POINT('',#17786);
#5156=VERTEX_POINT('',#17788);
#5157=VERTEX_POINT('',#17792);
#5158=VERTEX_POINT('',#17793);
#5159=VERTEX_POINT('',#17795);
#5160=VERTEX_POINT('',#17797);
#5161=VERTEX_POINT('',#17801);
#5162=VERTEX_POINT('',#17803);
#5163=VERTEX_POINT('',#17806);
#5164=VERTEX_POINT('',#17808);
#5165=VERTEX_POINT('',#17812);
#5166=VERTEX_POINT('',#17814);
#5167=VERTEX_POINT('',#17818);
#5168=VERTEX_POINT('',#17819);
#5169=VERTEX_POINT('',#17824);
#5170=VERTEX_POINT('',#17826);
#5171=VERTEX_POINT('',#17830);
#5172=VERTEX_POINT('',#17832);
#5173=VERTEX_POINT('',#17836);
#5174=VERTEX_POINT('',#17841);
#5175=VERTEX_POINT('',#17846);
#5176=VERTEX_POINT('',#17848);
#5177=VERTEX_POINT('',#17851);
#5178=VERTEX_POINT('',#17853);
#5179=VERTEX_POINT('',#17855);
#5180=VERTEX_POINT('',#17858);
#5181=VERTEX_POINT('',#17861);
#5182=VERTEX_POINT('',#17863);
#5183=VERTEX_POINT('',#17865);
#5184=VERTEX_POINT('',#17868);
#5185=VERTEX_POINT('',#17869);
#5186=VERTEX_POINT('',#17875);
#5187=VERTEX_POINT('',#17876);
#5188=VERTEX_POINT('',#17878);
#5189=VERTEX_POINT('',#17880);
#5190=VERTEX_POINT('',#17883);
#5191=VERTEX_POINT('',#17885);
#5192=VERTEX_POINT('',#17887);
#5193=VERTEX_POINT('',#17889);
#5194=VERTEX_POINT('',#17891);
#5195=VERTEX_POINT('',#17893);
#5196=VERTEX_POINT('',#17895);
#5197=VERTEX_POINT('',#17898);
#5198=VERTEX_POINT('',#17900);
#5199=VERTEX_POINT('',#17902);
#5200=VERTEX_POINT('',#17904);
#5201=VERTEX_POINT('',#17908);
#5202=VERTEX_POINT('',#17909);
#5203=VERTEX_POINT('',#17914);
#5204=VERTEX_POINT('',#17915);
#5205=VERTEX_POINT('',#17917);
#5206=VERTEX_POINT('',#17919);
#5207=VERTEX_POINT('',#17923);
#5208=VERTEX_POINT('',#17925);
#5209=VERTEX_POINT('',#17929);
#5210=VERTEX_POINT('',#17931);
#5211=VERTEX_POINT('',#17933);
#5212=VERTEX_POINT('',#17935);
#5213=VERTEX_POINT('',#17937);
#5214=VERTEX_POINT('',#17939);
#5215=VERTEX_POINT('',#17941);
#5216=VERTEX_POINT('',#17943);
#5217=VERTEX_POINT('',#17945);
#5218=VERTEX_POINT('',#17947);
#5219=VERTEX_POINT('',#17949);
#5220=VERTEX_POINT('',#17952);
#5221=VERTEX_POINT('',#17954);
#5222=VERTEX_POINT('',#17957);
#5223=VERTEX_POINT('',#17959);
#5224=VERTEX_POINT('',#17961);
#5225=VERTEX_POINT('',#17963);
#5226=VERTEX_POINT('',#17981);
#5227=VERTEX_POINT('',#17982);
#5228=VERTEX_POINT('',#17988);
#5229=VERTEX_POINT('',#17989);
#5230=VERTEX_POINT('',#17995);
#5231=VERTEX_POINT('',#17997);
#5232=VERTEX_POINT('',#17999);
#5233=VERTEX_POINT('',#18003);
#5234=VERTEX_POINT('',#18004);
#5235=VERTEX_POINT('',#18009);
#5236=VERTEX_POINT('',#18010);
#5237=VERTEX_POINT('',#18015);
#5238=VERTEX_POINT('',#18019);
#5239=VERTEX_POINT('',#18021);
#5240=VERTEX_POINT('',#18025);
#5241=VERTEX_POINT('',#18026);
#5242=VERTEX_POINT('',#18028);
#5243=VERTEX_POINT('',#18030);
#5244=VERTEX_POINT('',#18035);
#5245=VERTEX_POINT('',#18037);
#5246=VERTEX_POINT('',#18041);
#5247=VERTEX_POINT('',#18046);
#5248=VERTEX_POINT('',#18050);
#5249=VERTEX_POINT('',#18051);
#5250=VERTEX_POINT('',#18053);
#5251=VERTEX_POINT('',#18055);
#5252=VERTEX_POINT('',#18059);
#5253=VERTEX_POINT('',#18061);
#5254=VERTEX_POINT('',#18075);
#5255=VERTEX_POINT('',#18076);
#5256=VERTEX_POINT('',#18078);
#5257=VERTEX_POINT('',#18080);
#5258=VERTEX_POINT('',#18084);
#5259=VERTEX_POINT('',#18085);
#5260=VERTEX_POINT('',#18087);
#5261=VERTEX_POINT('',#18089);
#5262=VERTEX_POINT('',#18094);
#5263=VERTEX_POINT('',#18099);
#5264=VERTEX_POINT('',#18100);
#5265=VERTEX_POINT('',#18102);
#5266=VERTEX_POINT('',#18104);
#5267=VERTEX_POINT('',#18108);
#5268=VERTEX_POINT('',#18114);
#5269=VERTEX_POINT('',#18123);
#5270=VERTEX_POINT('',#18125);
#5271=VERTEX_POINT('',#18129);
#5272=VERTEX_POINT('',#18133);
#5273=VERTEX_POINT('',#18137);
#5274=VERTEX_POINT('',#18138);
#5275=VERTEX_POINT('',#18143);
#5276=VERTEX_POINT('',#18145);
#5277=VERTEX_POINT('',#18150);
#5278=VERTEX_POINT('',#18160);
#5279=VERTEX_POINT('',#18162);
#5280=VERTEX_POINT('',#18164);
#5281=VERTEX_POINT('',#18169);
#5282=VERTEX_POINT('',#18183);
#5283=VERTEX_POINT('',#18184);
#5284=VERTEX_POINT('',#18186);
#5285=VERTEX_POINT('',#18188);
#5286=VERTEX_POINT('',#18192);
#5287=VERTEX_POINT('',#18198);
#5288=VERTEX_POINT('',#18200);
#5289=VERTEX_POINT('',#18204);
#5290=VERTEX_POINT('',#18219);
#5291=VERTEX_POINT('',#18220);
#5292=VERTEX_POINT('',#18222);
#5293=VERTEX_POINT('',#18224);
#5294=VERTEX_POINT('',#18230);
#5295=VERTEX_POINT('',#18231);
#5296=VERTEX_POINT('',#18233);
#5297=VERTEX_POINT('',#18235);
#5298=VERTEX_POINT('',#18239);
#5299=VERTEX_POINT('',#18241);
#5300=VERTEX_POINT('',#18244);
#5301=VERTEX_POINT('',#18246);
#5302=VERTEX_POINT('',#18250);
#5303=VERTEX_POINT('',#18251);
#5304=VERTEX_POINT('',#18254);
#5305=VERTEX_POINT('',#18256);
#5306=VERTEX_POINT('',#18473);
#5307=VERTEX_POINT('',#18474);
#5308=VERTEX_POINT('',#18476);
#5309=VERTEX_POINT('',#18478);
#5310=VERTEX_POINT('',#18482);
#5311=VERTEX_POINT('',#18484);
#5312=VERTEX_POINT('',#18486);
#5313=VERTEX_POINT('',#18488);
#5314=VERTEX_POINT('',#18490);
#5315=VERTEX_POINT('',#18492);
#5316=VERTEX_POINT('',#18494);
#5317=VERTEX_POINT('',#18496);
#5318=VERTEX_POINT('',#18498);
#5319=VERTEX_POINT('',#18500);
#5320=VERTEX_POINT('',#18502);
#5321=VERTEX_POINT('',#18505);
#5322=VERTEX_POINT('',#18507);
#5323=VERTEX_POINT('',#18510);
#5324=VERTEX_POINT('',#18514);
#5325=VERTEX_POINT('',#18515);
#5326=VERTEX_POINT('',#18517);
#5327=VERTEX_POINT('',#18519);
#5328=VERTEX_POINT('',#18523);
#5329=VERTEX_POINT('',#18525);
#5330=VERTEX_POINT('',#18527);
#5331=VERTEX_POINT('',#18529);
#5332=VERTEX_POINT('',#18531);
#5333=VERTEX_POINT('',#18533);
#5334=VERTEX_POINT('',#18535);
#5335=VERTEX_POINT('',#18537);
#5336=VERTEX_POINT('',#18539);
#5337=VERTEX_POINT('',#18541);
#5338=VERTEX_POINT('',#18543);
#5339=VERTEX_POINT('',#18545);
#5340=VERTEX_POINT('',#18547);
#5341=VERTEX_POINT('',#18550);
#5342=VERTEX_POINT('',#18552);
#5343=VERTEX_POINT('',#18554);
#5344=VERTEX_POINT('',#18557);
#5345=VERTEX_POINT('',#18561);
#5346=VERTEX_POINT('',#18565);
#5347=VERTEX_POINT('',#18569);
#5348=VERTEX_POINT('',#18573);
#5349=VERTEX_POINT('',#18577);
#5350=VERTEX_POINT('',#18579);
#5351=VERTEX_POINT('',#18590);
#5352=VERTEX_POINT('',#18592);
#5353=VERTEX_POINT('',#18594);
#5354=VERTEX_POINT('',#18596);
#5355=VERTEX_POINT('',#18598);
#5356=VERTEX_POINT('',#18600);
#5357=VERTEX_POINT('',#18602);
#5358=VERTEX_POINT('',#18605);
#5359=VERTEX_POINT('',#18607);
#5360=VERTEX_POINT('',#18610);
#5361=VERTEX_POINT('',#18612);
#5362=VERTEX_POINT('',#18619);
#5363=VERTEX_POINT('',#18621);
#5364=VERTEX_POINT('',#18625);
#5365=VERTEX_POINT('',#18626);
#5366=VERTEX_POINT('',#18629);
#5367=VERTEX_POINT('',#18633);
#5368=VERTEX_POINT('',#18635);
#5369=VERTEX_POINT('',#18642);
#5370=VERTEX_POINT('',#18644);
#5371=VERTEX_POINT('',#18659);
#5372=VERTEX_POINT('',#18664);
#5373=VERTEX_POINT('',#18668);
#5374=VERTEX_POINT('',#18672);
#5375=VERTEX_POINT('',#18676);
#5376=VERTEX_POINT('',#18678);
#5377=VERTEX_POINT('',#18685);
#5378=VERTEX_POINT('',#18686);
#5379=VERTEX_POINT('',#18688);
#5380=VERTEX_POINT('',#18690);
#5381=VERTEX_POINT('',#18694);
#5382=VERTEX_POINT('',#18703);
#5383=VERTEX_POINT('',#18716);
#5384=VERTEX_POINT('',#18718);
#5385=VERTEX_POINT('',#18722);
#5386=VERTEX_POINT('',#18723);
#5387=VERTEX_POINT('',#18735);
#5388=VERTEX_POINT('',#18737);
#5389=VERTEX_POINT('',#18754);
#5390=VERTEX_POINT('',#18758);
#5391=VERTEX_POINT('',#18771);
#5392=VERTEX_POINT('',#18773);
#5393=VERTEX_POINT('',#18792);
#5394=VERTEX_POINT('',#18794);
#5395=VERTEX_POINT('',#18798);
#5396=VERTEX_POINT('',#18800);
#5397=VERTEX_POINT('',#18804);
#5398=VERTEX_POINT('',#18805);
#5399=VERTEX_POINT('',#18808);
#5400=VERTEX_POINT('',#18812);
#5401=VERTEX_POINT('',#18821);
#5402=VERTEX_POINT('',#18823);
#5403=VERTEX_POINT('',#18827);
#5404=VERTEX_POINT('',#18829);
#5405=VERTEX_POINT('',#18833);
#5406=VERTEX_POINT('',#18834);
#5407=VERTEX_POINT('',#18836);
#5408=VERTEX_POINT('',#18841);
#5409=VERTEX_POINT('',#18854);
#5410=VERTEX_POINT('',#18855);
#5411=VERTEX_POINT('',#18858);
#5412=VERTEX_POINT('',#18862);
#5413=VERTEX_POINT('',#18863);
#5414=VERTEX_POINT('',#18865);
#5415=VERTEX_POINT('',#18869);
#5416=VERTEX_POINT('',#18875);
#5417=VERTEX_POINT('',#18876);
#5418=VERTEX_POINT('',#18878);
#5419=VERTEX_POINT('',#18880);
#5420=VERTEX_POINT('',#18882);
#5421=VERTEX_POINT('',#18884);
#5422=VERTEX_POINT('',#18886);
#5423=VERTEX_POINT('',#18888);
#5424=VERTEX_POINT('',#18890);
#5425=VERTEX_POINT('',#18892);
#5426=VERTEX_POINT('',#18894);
#5427=VERTEX_POINT('',#18896);
#5428=VERTEX_POINT('',#18898);
#5429=VERTEX_POINT('',#18900);
#5430=VERTEX_POINT('',#18902);
#5431=VERTEX_POINT('',#18904);
#5432=VERTEX_POINT('',#18908);
#5433=VERTEX_POINT('',#18909);
#5434=VERTEX_POINT('',#18911);
#5435=VERTEX_POINT('',#18913);
#5436=VERTEX_POINT('',#18916);
#5437=VERTEX_POINT('',#18918);
#5438=VERTEX_POINT('',#18920);
#5439=VERTEX_POINT('',#18922);
#5440=VERTEX_POINT('',#18924);
#5441=VERTEX_POINT('',#18926);
#5442=VERTEX_POINT('',#18928);
#5443=VERTEX_POINT('',#18930);
#5444=VERTEX_POINT('',#18932);
#5445=VERTEX_POINT('',#18934);
#5446=VERTEX_POINT('',#18937);
#5447=VERTEX_POINT('',#18942);
#5448=VERTEX_POINT('',#18946);
#5449=VERTEX_POINT('',#18952);
#5450=VERTEX_POINT('',#18956);
#5451=VERTEX_POINT('',#18962);
#5452=VERTEX_POINT('',#18966);
#5453=VERTEX_POINT('',#18973);
#5454=VERTEX_POINT('',#18977);
#5455=VERTEX_POINT('',#18983);
#5456=VERTEX_POINT('',#18985);
#5457=VERTEX_POINT('',#19000);
#5458=VERTEX_POINT('',#19007);
#5459=VERTEX_POINT('',#19023);
#5460=VERTEX_POINT('',#19030);
#5461=VERTEX_POINT('',#19046);
#5462=VERTEX_POINT('',#19048);
#5463=VERTEX_POINT('',#19052);
#5464=VERTEX_POINT('',#19054);
#5465=VERTEX_POINT('',#19056);
#5466=VERTEX_POINT('',#19060);
#5467=VERTEX_POINT('',#19062);
#5468=VERTEX_POINT('',#19064);
#5469=VERTEX_POINT('',#19070);
#5470=VERTEX_POINT('',#19072);
#5471=VERTEX_POINT('',#19076);
#5472=VERTEX_POINT('',#19077);
#5473=VERTEX_POINT('',#19092);
#5474=VERTEX_POINT('',#19094);
#5475=VERTEX_POINT('',#19103);
#5476=VERTEX_POINT('',#19106);
#5477=VERTEX_POINT('',#19117);
#5478=VERTEX_POINT('',#19119);
#5479=VERTEX_POINT('',#19123);
#5480=VERTEX_POINT('',#19127);
#5481=VERTEX_POINT('',#19129);
#5482=VERTEX_POINT('',#19133);
#5483=VERTEX_POINT('',#19135);
#5484=VERTEX_POINT('',#19139);
#5485=VERTEX_POINT('',#19140);
#5486=VERTEX_POINT('',#19142);
#5487=VERTEX_POINT('',#19144);
#5488=VERTEX_POINT('',#19148);
#5489=VERTEX_POINT('',#19150);
#5490=VERTEX_POINT('',#19154);
#5491=VERTEX_POINT('',#19155);
#5492=VERTEX_POINT('',#19157);
#5493=VERTEX_POINT('',#19159);
#5494=VERTEX_POINT('',#19163);
#5495=VERTEX_POINT('',#19165);
#5496=VERTEX_POINT('',#19167);
#5497=VERTEX_POINT('',#19169);
#5498=VERTEX_POINT('',#19173);
#5499=VERTEX_POINT('',#19177);
#5500=VERTEX_POINT('',#19179);
#5501=VERTEX_POINT('',#19181);
#5502=VERTEX_POINT('',#19185);
#5503=VERTEX_POINT('',#19187);
#5504=VERTEX_POINT('',#19191);
#5505=VERTEX_POINT('',#19193);
#5506=VERTEX_POINT('',#19197);
#5507=VERTEX_POINT('',#19199);
#5508=VERTEX_POINT('',#19201);
#5509=VERTEX_POINT('',#19203);
#5510=VERTEX_POINT('',#19205);
#5511=VERTEX_POINT('',#19207);
#5512=VERTEX_POINT('',#19211);
#5513=VERTEX_POINT('',#19212);
#5514=VERTEX_POINT('',#19215);
#5515=VERTEX_POINT('',#19217);
#5516=VERTEX_POINT('',#19221);
#5517=VERTEX_POINT('',#19222);
#5518=VERTEX_POINT('',#19224);
#5519=VERTEX_POINT('',#19226);
#5520=VERTEX_POINT('',#19230);
#5521=VERTEX_POINT('',#19231);
#5522=VERTEX_POINT('',#19236);
#5523=VERTEX_POINT('',#19238);
#5524=VERTEX_POINT('',#19241);
#5525=VERTEX_POINT('',#19243);
#5526=VERTEX_POINT('',#19247);
#5527=VERTEX_POINT('',#19251);
#5528=VERTEX_POINT('',#19255);
#5529=VERTEX_POINT('',#19256);
#5530=VERTEX_POINT('',#19261);
#5531=VERTEX_POINT('',#19263);
#5532=VERTEX_POINT('',#19266);
#5533=VERTEX_POINT('',#19268);
#5534=VERTEX_POINT('',#19297);
#5535=VERTEX_POINT('',#19299);
#5536=VERTEX_POINT('',#19303);
#5537=VERTEX_POINT('',#19304);
#5538=VERTEX_POINT('',#19307);
#5539=VERTEX_POINT('',#19315);
#5540=VERTEX_POINT('',#19317);
#5541=VERTEX_POINT('',#19321);
#5542=VERTEX_POINT('',#19322);
#5543=VERTEX_POINT('',#19325);
#5544=VERTEX_POINT('',#19337);
#5545=VERTEX_POINT('',#19339);
#5546=VERTEX_POINT('',#19343);
#5547=VERTEX_POINT('',#19345);
#5548=VERTEX_POINT('',#19349);
#5549=VERTEX_POINT('',#19350);
#5550=VERTEX_POINT('',#19352);
#5551=VERTEX_POINT('',#19354);
#5552=VERTEX_POINT('',#19356);
#5553=VERTEX_POINT('',#19358);
#5554=VERTEX_POINT('',#19360);
#5555=VERTEX_POINT('',#19362);
#5556=VERTEX_POINT('',#19366);
#5557=VERTEX_POINT('',#19367);
#5558=VERTEX_POINT('',#19369);
#5559=VERTEX_POINT('',#19371);
#5560=VERTEX_POINT('',#19373);
#5561=VERTEX_POINT('',#19375);
#5562=VERTEX_POINT('',#19377);
#5563=VERTEX_POINT('',#19379);
#5564=VERTEX_POINT('',#19401);
#5565=VERTEX_POINT('',#19402);
#5566=VERTEX_POINT('',#19421);
#5567=VERTEX_POINT('',#19443);
#5568=VERTEX_POINT('',#19445);
#5569=VERTEX_POINT('',#19447);
#5570=VERTEX_POINT('',#19451);
#5571=VERTEX_POINT('',#19452);
#5572=VERTEX_POINT('',#19455);
#5573=VERTEX_POINT('',#19459);
#5574=VERTEX_POINT('',#19461);
#5575=VERTEX_POINT('',#19465);
#5576=VERTEX_POINT('',#19467);
#5577=VERTEX_POINT('',#19471);
#5578=VERTEX_POINT('',#19473);
#5579=VERTEX_POINT('',#19477);
#5580=VERTEX_POINT('',#19479);
#5581=VERTEX_POINT('',#19483);
#5582=VERTEX_POINT('',#19484);
#5583=VERTEX_POINT('',#19486);
#5584=VERTEX_POINT('',#19488);
#5585=VERTEX_POINT('',#19490);
#5586=VERTEX_POINT('',#19492);
#5587=VERTEX_POINT('',#19494);
#5588=VERTEX_POINT('',#19498);
#5589=VERTEX_POINT('',#19499);
#5590=VERTEX_POINT('',#19501);
#5591=VERTEX_POINT('',#19503);
#5592=VERTEX_POINT('',#19505);
#5593=VERTEX_POINT('',#19507);
#5594=VERTEX_POINT('',#19509);
#5595=VERTEX_POINT('',#19513);
#5596=VERTEX_POINT('',#19515);
#5597=VERTEX_POINT('',#19517);
#5598=VERTEX_POINT('',#19519);
#5599=VERTEX_POINT('',#19521);
#5600=VERTEX_POINT('',#19523);
#5601=VERTEX_POINT('',#19525);
#5602=VERTEX_POINT('',#19529);
#5603=VERTEX_POINT('',#19530);
#5604=VERTEX_POINT('',#19532);
#5605=VERTEX_POINT('',#19534);
#5606=VERTEX_POINT('',#19538);
#5607=VERTEX_POINT('',#19540);
#5608=VERTEX_POINT('',#19544);
#5609=VERTEX_POINT('',#19546);
#5610=VERTEX_POINT('',#19550);
#5611=VERTEX_POINT('',#19552);
#5612=VERTEX_POINT('',#19556);
#5613=VERTEX_POINT('',#19558);
#5614=VERTEX_POINT('',#19560);
#5615=VERTEX_POINT('',#19562);
#5616=VERTEX_POINT('',#19566);
#5617=VERTEX_POINT('',#19567);
#5618=VERTEX_POINT('',#19572);
#5619=VERTEX_POINT('',#19574);
#5620=VERTEX_POINT('',#19576);
#5621=VERTEX_POINT('',#19578);
#5622=VERTEX_POINT('',#19580);
#5623=VERTEX_POINT('',#19588);
#5624=VERTEX_POINT('',#19590);
#5625=VERTEX_POINT('',#19613);
#5626=VERTEX_POINT('',#19681);
#5627=VERTEX_POINT('',#19683);
#5628=VERTEX_POINT('',#19751);
#5629=VERTEX_POINT('',#19759);
#5630=VERTEX_POINT('',#19776);
#5631=VERTEX_POINT('',#19841);
#5632=VERTEX_POINT('',#19843);
#5633=VERTEX_POINT('',#19933);
#5634=VERTEX_POINT('',#19934);
#5635=VERTEX_POINT('',#19936);
#5636=VERTEX_POINT('',#19938);
#5637=VERTEX_POINT('',#19942);
#5638=VERTEX_POINT('',#19943);
#5639=VERTEX_POINT('',#20038);
#5640=VERTEX_POINT('',#20039);
#5641=VERTEX_POINT('',#20055);
#5642=VERTEX_POINT('',#20056);
#5643=VERTEX_POINT('',#20058);
#5644=VERTEX_POINT('',#20060);
#5645=VERTEX_POINT('',#20062);
#5646=VERTEX_POINT('',#20064);
#5647=VERTEX_POINT('',#20068);
#5648=VERTEX_POINT('',#20070);
#5649=VERTEX_POINT('',#20074);
#5650=VERTEX_POINT('',#20078);
#5651=VERTEX_POINT('',#20082);
#5652=VERTEX_POINT('',#20086);
#5653=VERTEX_POINT('',#20092);
#5654=VERTEX_POINT('',#20093);
#5655=VERTEX_POINT('',#20095);
#5656=VERTEX_POINT('',#20097);
#5657=VERTEX_POINT('',#20099);
#5658=VERTEX_POINT('',#20101);
#5659=VERTEX_POINT('',#20105);
#5660=VERTEX_POINT('',#20106);
#5661=VERTEX_POINT('',#20108);
#5662=VERTEX_POINT('',#20110);
#5663=VERTEX_POINT('',#20112);
#5664=VERTEX_POINT('',#20115);
#5665=VERTEX_POINT('',#20120);
#5666=VERTEX_POINT('',#20122);
#5667=VERTEX_POINT('',#20132);
#5668=VERTEX_POINT('',#20134);
#5669=VERTEX_POINT('',#20138);
#5670=VERTEX_POINT('',#20142);
#5671=VERTEX_POINT('',#20148);
#5672=VERTEX_POINT('',#20152);
#5673=VERTEX_POINT('',#20156);
#5674=VERTEX_POINT('',#20160);
#5675=VERTEX_POINT('',#20164);
#5676=VERTEX_POINT('',#20168);
#5677=VERTEX_POINT('',#20172);
#5678=VERTEX_POINT('',#20174);
#5679=VERTEX_POINT('',#20179);
#5680=VERTEX_POINT('',#20181);
#5681=VERTEX_POINT('',#20185);
#5682=VERTEX_POINT('',#20186);
#5683=VERTEX_POINT('',#20189);
#5684=VERTEX_POINT('',#20193);
#5685=VERTEX_POINT('',#20198);
#5686=VERTEX_POINT('',#20200);
#5687=VERTEX_POINT('',#20204);
#5688=VERTEX_POINT('',#20206);
#5689=VERTEX_POINT('',#20210);
#5690=VERTEX_POINT('',#20213);
#5691=VERTEX_POINT('',#20221);
#5692=VERTEX_POINT('',#20225);
#5693=VERTEX_POINT('',#20239);
#5694=VERTEX_POINT('',#20240);
#5695=VERTEX_POINT('',#20246);
#5696=VERTEX_POINT('',#20331);
#5697=VERTEX_POINT('',#20333);
#5698=VERTEX_POINT('',#20338);
#5699=VERTEX_POINT('',#21131);
#5700=VERTEX_POINT('',#21132);
#5701=VERTEX_POINT('',#21134);
#5702=VERTEX_POINT('',#21145);
#5703=VERTEX_POINT('',#21147);
#5704=VERTEX_POINT('',#21150);
#5705=VERTEX_POINT('',#21163);
#5706=VERTEX_POINT('',#21180);
#5707=VERTEX_POINT('',#21201);
#5708=VERTEX_POINT('',#21203);
#5709=VERTEX_POINT('',#21239);
#5710=VERTEX_POINT('',#21240);
#5711=VERTEX_POINT('',#21242);
#5712=VERTEX_POINT('',#21244);
#5713=VERTEX_POINT('',#21249);
#5714=VERTEX_POINT('',#21260);
#5715=VERTEX_POINT('',#21262);
#5716=VERTEX_POINT('',#21266);
#5717=VERTEX_POINT('',#21268);
#5718=VERTEX_POINT('',#21272);
#5719=VERTEX_POINT('',#21274);
#5720=VERTEX_POINT('',#21278);
#5721=VERTEX_POINT('',#21280);
#5722=VERTEX_POINT('',#21284);
#5723=VERTEX_POINT('',#21286);
#5724=VERTEX_POINT('',#21297);
#5725=VERTEX_POINT('',#21302);
#5726=VERTEX_POINT('',#21303);
#5727=VERTEX_POINT('',#21305);
#5728=VERTEX_POINT('',#21307);
#5729=VERTEX_POINT('',#21309);
#5730=VERTEX_POINT('',#21311);
#5731=VERTEX_POINT('',#21313);
#5732=VERTEX_POINT('',#21315);
#5733=VERTEX_POINT('',#21319);
#5734=VERTEX_POINT('',#21320);
#5735=VERTEX_POINT('',#21322);
#5736=VERTEX_POINT('',#21324);
#5737=VERTEX_POINT('',#21326);
#5738=VERTEX_POINT('',#21328);
#5739=VERTEX_POINT('',#21330);
#5740=VERTEX_POINT('',#21332);
#5741=VERTEX_POINT('',#21337);
#5742=VERTEX_POINT('',#21339);
#5743=VERTEX_POINT('',#21341);
#5744=VERTEX_POINT('',#21343);
#5745=VERTEX_POINT('',#21345);
#5746=VERTEX_POINT('',#21347);
#5747=VERTEX_POINT('',#21349);
#5748=VERTEX_POINT('',#21351);
#5749=VERTEX_POINT('',#21353);
#5750=VERTEX_POINT('',#21355);
#5751=VERTEX_POINT('',#21357);
#5752=VERTEX_POINT('',#21359);
#5753=VERTEX_POINT('',#21361);
#5754=VERTEX_POINT('',#21363);
#5755=VERTEX_POINT('',#21365);
#5756=VERTEX_POINT('',#21367);
#5757=VERTEX_POINT('',#21371);
#5758=VERTEX_POINT('',#21372);
#5759=VERTEX_POINT('',#21374);
#5760=VERTEX_POINT('',#21376);
#5761=VERTEX_POINT('',#21378);
#5762=VERTEX_POINT('',#21380);
#5763=VERTEX_POINT('',#21382);
#5764=VERTEX_POINT('',#21384);
#5765=VERTEX_POINT('',#21386);
#5766=VERTEX_POINT('',#21388);
#5767=VERTEX_POINT('',#21392);
#5768=VERTEX_POINT('',#21394);
#5769=VERTEX_POINT('',#21396);
#5770=VERTEX_POINT('',#21398);
#5771=VERTEX_POINT('',#21400);
#5772=VERTEX_POINT('',#21402);
#5773=VERTEX_POINT('',#21420);
#5774=VERTEX_POINT('',#21422);
#5775=VERTEX_POINT('',#21424);
#5776=VERTEX_POINT('',#21426);
#5777=VERTEX_POINT('',#21444);
#5778=VERTEX_POINT('',#21445);
#5779=VERTEX_POINT('',#21448);
#5780=VERTEX_POINT('',#21450);
#5781=VERTEX_POINT('',#21508);
#5782=VERTEX_POINT('',#21509);
#5783=VERTEX_POINT('',#21548);
#5784=VERTEX_POINT('',#21550);
#5785=VERTEX_POINT('',#21610);
#5786=VERTEX_POINT('',#21611);
#5787=VERTEX_POINT('',#21650);
#5788=VERTEX_POINT('',#21652);
#5789=VERTEX_POINT('',#21756);
#5790=VERTEX_POINT('',#21761);
#5791=VERTEX_POINT('',#21811);
#5792=VERTEX_POINT('',#21815);
#5793=VERTEX_POINT('',#21816);
#5794=VERTEX_POINT('',#21819);
#5795=VERTEX_POINT('',#21823);
#5796=VERTEX_POINT('',#21937);
#5797=VERTEX_POINT('',#21938);
#5798=VERTEX_POINT('',#21977);
#5799=VERTEX_POINT('',#21979);
#5800=VERTEX_POINT('',#22039);
#5801=VERTEX_POINT('',#22040);
#5802=VERTEX_POINT('',#22079);
#5803=VERTEX_POINT('',#22081);
#5804=VERTEX_POINT('',#22185);
#5805=VERTEX_POINT('',#22190);
#5806=VERTEX_POINT('',#22240);
#5807=VERTEX_POINT('',#22244);
#5808=VERTEX_POINT('',#22245);
#5809=VERTEX_POINT('',#22248);
#5810=VERTEX_POINT('',#22252);
#5811=VERTEX_POINT('',#22332);
#5812=VERTEX_POINT('',#22334);
#5813=VERTEX_POINT('',#22338);
#5814=VERTEX_POINT('',#22340);
#5815=VERTEX_POINT('',#22344);
#5816=VERTEX_POINT('',#22345);
#5817=VERTEX_POINT('',#22348);
#5818=VERTEX_POINT('',#22351);
#5819=VERTEX_POINT('',#22352);
#5820=VERTEX_POINT('',#22355);
#5821=VERTEX_POINT('',#22358);
#5822=VERTEX_POINT('',#22360);
#5823=VERTEX_POINT('',#22364);
#5824=VERTEX_POINT('',#22369);
#5825=VERTEX_POINT('',#22371);
#5826=VERTEX_POINT('',#22375);
#5827=VERTEX_POINT('',#22436);
#5828=VERTEX_POINT('',#22438);
#5829=VERTEX_POINT('',#22442);
#5830=VERTEX_POINT('',#22444);
#5831=VERTEX_POINT('',#22448);
#5832=VERTEX_POINT('',#22449);
#5833=VERTEX_POINT('',#22452);
#5834=VERTEX_POINT('',#22455);
#5835=VERTEX_POINT('',#22456);
#5836=VERTEX_POINT('',#22458);
#5837=VERTEX_POINT('',#22462);
#5838=VERTEX_POINT('',#22464);
#5839=VERTEX_POINT('',#22468);
#5840=VERTEX_POINT('',#22473);
#5841=VERTEX_POINT('',#22475);
#5842=VERTEX_POINT('',#22479);
#5843=VERTEX_POINT('',#22549);
#5844=VERTEX_POINT('',#22551);
#5845=VERTEX_POINT('',#22555);
#5846=VERTEX_POINT('',#22557);
#5847=VERTEX_POINT('',#22561);
#5848=VERTEX_POINT('',#22563);
#5849=VERTEX_POINT('',#22567);
#5850=VERTEX_POINT('',#22569);
#5851=VERTEX_POINT('',#22573);
#5852=VERTEX_POINT('',#22575);
#5853=VERTEX_POINT('',#22577);
#5854=VERTEX_POINT('',#22579);
#5855=VERTEX_POINT('',#22581);
#5856=VERTEX_POINT('',#22583);
#5857=VERTEX_POINT('',#22585);
#5858=VERTEX_POINT('',#22587);
#5859=VERTEX_POINT('',#22589);
#5860=VERTEX_POINT('',#22591);
#5861=VERTEX_POINT('',#22595);
#5862=VERTEX_POINT('',#22596);
#5863=VERTEX_POINT('',#22598);
#5864=VERTEX_POINT('',#22612);
#5865=VERTEX_POINT('',#22614);
#5866=VERTEX_POINT('',#22616);
#5867=VERTEX_POINT('',#22618);
#5868=VERTEX_POINT('',#22620);
#5869=VERTEX_POINT('',#22622);
#5870=VERTEX_POINT('',#22625);
#5871=VERTEX_POINT('',#22627);
#5872=VERTEX_POINT('',#22629);
#5873=VERTEX_POINT('',#22631);
#5874=VERTEX_POINT('',#22633);
#5875=VERTEX_POINT('',#22649);
#5876=VERTEX_POINT('',#22652);
#5877=VERTEX_POINT('',#22657);
#5878=VERTEX_POINT('',#22659);
#5879=VERTEX_POINT('',#22667);
#5880=VERTEX_POINT('',#22669);
#5881=VERTEX_POINT('',#22673);
#5882=VERTEX_POINT('',#22675);
#5883=VERTEX_POINT('',#22679);
#5884=VERTEX_POINT('',#22681);
#5885=VERTEX_POINT('',#22690);
#5886=VERTEX_POINT('',#22692);
#5887=VERTEX_POINT('',#22696);
#5888=VERTEX_POINT('',#22698);
#5889=VERTEX_POINT('',#22702);
#5890=VERTEX_POINT('',#22704);
#5891=VERTEX_POINT('',#23165);
#5892=VERTEX_POINT('',#23166);
#5893=VERTEX_POINT('',#23169);
#5894=VERTEX_POINT('',#23171);
#5895=VERTEX_POINT('',#23175);
#5896=VERTEX_POINT('',#23179);
#5897=VERTEX_POINT('',#23185);
#5898=VERTEX_POINT('',#23187);
#5899=VERTEX_POINT('',#23189);
#5900=VERTEX_POINT('',#23193);
#5901=VERTEX_POINT('',#23194);
#5902=VERTEX_POINT('',#23197);
#5903=VERTEX_POINT('',#23203);
#5904=VERTEX_POINT('',#23205);
#5905=VERTEX_POINT('',#23217);
#5906=VERTEX_POINT('',#23219);
#5907=VERTEX_POINT('',#23223);
#5908=VERTEX_POINT('',#23224);
#5909=VERTEX_POINT('',#23227);
#5910=VERTEX_POINT('',#23236);
#5911=VERTEX_POINT('',#23237);
#5912=VERTEX_POINT('',#23240);
#5913=VERTEX_POINT('',#23244);
#5914=VERTEX_POINT('',#23246);
#5915=VERTEX_POINT('',#23250);
#5916=VERTEX_POINT('',#23252);
#5917=VERTEX_POINT('',#23254);
#5918=VERTEX_POINT('',#23258);
#5919=VERTEX_POINT('',#23260);
#5920=VERTEX_POINT('',#23264);
#5921=VERTEX_POINT('',#23265);
#5922=VERTEX_POINT('',#23268);
#5923=VERTEX_POINT('',#23272);
#5924=VERTEX_POINT('',#23274);
#5925=VERTEX_POINT('',#23276);
#5926=VERTEX_POINT('',#23280);
#5927=VERTEX_POINT('',#23282);
#5928=VERTEX_POINT('',#23286);
#5929=VERTEX_POINT('',#23288);
#5930=VERTEX_POINT('',#23294);
#5931=VERTEX_POINT('',#23296);
#5932=VERTEX_POINT('',#23314);
#5933=VERTEX_POINT('',#23315);
#5934=VERTEX_POINT('',#23318);
#5935=VERTEX_POINT('',#23322);
#5936=VERTEX_POINT('',#23324);
#5937=VERTEX_POINT('',#23328);
#5938=VERTEX_POINT('',#23330);
#5939=VERTEX_POINT('',#23332);
#5940=VERTEX_POINT('',#23336);
#5941=VERTEX_POINT('',#23338);
#5942=VERTEX_POINT('',#23342);
#5943=VERTEX_POINT('',#23343);
#5944=VERTEX_POINT('',#23346);
#5945=VERTEX_POINT('',#23350);
#5946=VERTEX_POINT('',#23352);
#5947=VERTEX_POINT('',#23354);
#5948=VERTEX_POINT('',#23358);
#5949=VERTEX_POINT('',#23360);
#5950=VERTEX_POINT('',#23364);
#5951=VERTEX_POINT('',#23366);
#5952=VERTEX_POINT('',#23372);
#5953=VERTEX_POINT('',#23374);
#5954=VERTEX_POINT('',#23388);
#5955=VERTEX_POINT('',#23390);
#5956=VERTEX_POINT('',#23394);
#5957=VERTEX_POINT('',#23395);
#5958=VERTEX_POINT('',#23398);
#5959=VERTEX_POINT('',#23406);
#5960=VERTEX_POINT('',#23407);
#5961=VERTEX_POINT('',#23409);
#5962=VERTEX_POINT('',#23419);
#5963=VERTEX_POINT('',#23431);
#5964=VERTEX_POINT('',#23432);
#5965=VERTEX_POINT('',#23469);
#5966=VERTEX_POINT('',#23470);
#5967=VERTEX_POINT('',#23507);
#5968=VERTEX_POINT('',#23508);
#5969=VERTEX_POINT('',#23545);
#5970=VERTEX_POINT('',#23546);
#5971=VERTEX_POINT('',#23583);
#5972=VERTEX_POINT('',#23584);
#5973=VERTEX_POINT('',#23621);
#5974=VERTEX_POINT('',#23622);
#5975=VERTEX_POINT('',#23659);
#5976=VERTEX_POINT('',#23660);
#5977=VERTEX_POINT('',#23697);
#5978=VERTEX_POINT('',#23698);
#5979=VERTEX_POINT('',#23735);
#5980=VERTEX_POINT('',#23736);
#5981=VERTEX_POINT('',#23773);
#5982=VERTEX_POINT('',#23774);
#5983=VERTEX_POINT('',#23811);
#5984=VERTEX_POINT('',#23812);
#5985=VERTEX_POINT('',#23849);
#5986=VERTEX_POINT('',#23850);
#5987=VERTEX_POINT('',#23887);
#5988=VERTEX_POINT('',#23888);
#5989=VERTEX_POINT('',#23890);
#5990=VERTEX_POINT('',#23927);
#5991=VERTEX_POINT('',#23930);
#5992=VERTEX_POINT('',#23959);
#5993=VERTEX_POINT('',#23990);
#5994=VERTEX_POINT('',#23991);
#5995=VERTEX_POINT('',#24066);
#5996=VERTEX_POINT('',#24067);
#5997=VERTEX_POINT('',#24144);
#5998=VERTEX_POINT('',#24145);
#5999=VERTEX_POINT('',#24220);
#6000=VERTEX_POINT('',#24221);
#6001=VERTEX_POINT('',#24296);
#6002=VERTEX_POINT('',#24297);
#6003=VERTEX_POINT('',#24372);
#6004=VERTEX_POINT('',#24373);
#6005=VERTEX_POINT('',#24448);
#6006=VERTEX_POINT('',#24449);
#6007=VERTEX_POINT('',#24524);
#6008=VERTEX_POINT('',#24525);
#6009=VERTEX_POINT('',#24602);
#6010=VERTEX_POINT('',#24603);
#6011=VERTEX_POINT('',#24678);
#6012=VERTEX_POINT('',#24679);
#6013=VERTEX_POINT('',#24754);
#6014=VERTEX_POINT('',#24755);
#6015=VERTEX_POINT('',#24830);
#6016=VERTEX_POINT('',#24843);
#6017=VERTEX_POINT('',#24854);
#6018=VERTEX_POINT('',#24856);
#6019=VERTEX_POINT('',#24858);
#6020=VERTEX_POINT('',#24860);
#6021=VERTEX_POINT('',#24862);
#6022=VERTEX_POINT('',#24866);
#6023=VERTEX_POINT('',#24868);
#6024=VERTEX_POINT('',#24872);
#6025=VERTEX_POINT('',#24874);
#6026=VERTEX_POINT('',#24878);
#6027=VERTEX_POINT('',#24891);
#6028=VERTEX_POINT('',#24894);
#6029=VERTEX_POINT('',#24921);
#6030=VERTEX_POINT('',#24936);
#6031=VERTEX_POINT('',#24937);
#6032=VERTEX_POINT('',#24942);
#6033=VERTEX_POINT('',#24946);
#6034=VERTEX_POINT('',#24947);
#6035=VERTEX_POINT('',#24949);
#6036=VERTEX_POINT('',#24951);
#6037=VERTEX_POINT('',#24955);
#6038=VERTEX_POINT('',#24956);
#6039=VERTEX_POINT('',#24958);
#6040=VERTEX_POINT('',#24960);
#6041=VERTEX_POINT('',#24964);
#6042=VERTEX_POINT('',#24968);
#6043=VERTEX_POINT('',#24969);
#6044=VERTEX_POINT('',#24971);
#6045=VERTEX_POINT('',#24973);
#6046=VERTEX_POINT('',#24977);
#6047=VERTEX_POINT('',#24978);
#6048=VERTEX_POINT('',#24980);
#6049=VERTEX_POINT('',#24982);
#6050=VERTEX_POINT('',#24986);
#6051=VERTEX_POINT('',#24987);
#6052=VERTEX_POINT('',#24989);
#6053=VERTEX_POINT('',#24991);
#6054=VERTEX_POINT('',#24995);
#6055=VERTEX_POINT('',#24998);
#6056=VERTEX_POINT('',#25002);
#6057=VERTEX_POINT('',#25005);
#6058=VERTEX_POINT('',#25955);
#6059=VERTEX_POINT('',#25956);
#6060=VERTEX_POINT('',#25958);
#6061=VERTEX_POINT('',#25974);
#6062=VERTEX_POINT('',#25994);
#6063=VERTEX_POINT('',#25995);
#6064=VERTEX_POINT('',#26032);
#6065=VERTEX_POINT('',#26033);
#6066=VERTEX_POINT('',#26070);
#6067=VERTEX_POINT('',#26071);
#6068=VERTEX_POINT('',#26108);
#6069=VERTEX_POINT('',#26109);
#6070=VERTEX_POINT('',#26146);
#6071=VERTEX_POINT('',#26147);
#6072=VERTEX_POINT('',#26184);
#6073=VERTEX_POINT('',#26185);
#6074=VERTEX_POINT('',#26222);
#6075=VERTEX_POINT('',#26223);
#6076=VERTEX_POINT('',#26225);
#6077=VERTEX_POINT('',#26235);
#6078=VERTEX_POINT('',#26247);
#6079=VERTEX_POINT('',#26248);
#6080=VERTEX_POINT('',#26250);
#6081=VERTEX_POINT('',#26269);
#6082=VERTEX_POINT('',#26271);
#6083=VERTEX_POINT('',#26292);
#6084=VERTEX_POINT('',#26332);
#6085=VERTEX_POINT('',#26333);
#6086=VERTEX_POINT('',#26410);
#6087=VERTEX_POINT('',#26411);
#6088=VERTEX_POINT('',#26486);
#6089=VERTEX_POINT('',#26487);
#6090=VERTEX_POINT('',#26562);
#6091=VERTEX_POINT('',#26563);
#6092=VERTEX_POINT('',#26638);
#6093=VERTEX_POINT('',#26639);
#6094=VERTEX_POINT('',#26714);
#6095=VERTEX_POINT('',#26715);
#6096=VERTEX_POINT('',#26790);
#6097=VERTEX_POINT('',#26791);
#6098=VERTEX_POINT('',#26793);
#6099=VERTEX_POINT('',#26806);
#6100=VERTEX_POINT('',#26902);
#6101=VERTEX_POINT('',#26904);
#6102=VERTEX_POINT('',#26908);
#6103=VERTEX_POINT('',#26909);
#6104=VERTEX_POINT('',#26911);
#6105=VERTEX_POINT('',#26913);
#6106=VERTEX_POINT('',#26915);
#6107=VERTEX_POINT('',#26917);
#6108=VERTEX_POINT('',#26919);
#6109=VERTEX_POINT('',#26921);
#6110=VERTEX_POINT('',#26923);
#6111=VERTEX_POINT('',#26925);
#6112=VERTEX_POINT('',#26927);
#6113=VERTEX_POINT('',#26929);
#6114=VERTEX_POINT('',#26961);
#6115=VERTEX_POINT('',#26962);
#6116=VERTEX_POINT('',#26964);
#6117=VERTEX_POINT('',#26966);
#6118=VERTEX_POINT('',#26968);
#6119=VERTEX_POINT('',#26970);
#6120=VERTEX_POINT('',#26975);
#6121=VERTEX_POINT('',#26977);
#6122=VERTEX_POINT('',#26983);
#6123=VERTEX_POINT('',#26987);
#6124=VERTEX_POINT('',#26993);
#6125=VERTEX_POINT('',#26997);
#6126=VERTEX_POINT('',#27694);
#6127=VERTEX_POINT('',#27696);
#6128=VERTEX_POINT('',#27700);
#6129=VERTEX_POINT('',#27701);
#6130=VERTEX_POINT('',#27704);
#6131=VERTEX_POINT('',#27708);
#6132=VERTEX_POINT('',#27712);
#6133=VERTEX_POINT('',#27720);
#6134=VERTEX_POINT('',#27722);
#6135=VERTEX_POINT('',#27726);
#6136=VERTEX_POINT('',#27727);
#6137=VERTEX_POINT('',#27730);
#6138=EDGE_CURVE('',#5035,#5035,#4394,.T.);
#6139=EDGE_CURVE('',#5035,#5036,#2754,.T.);
#6140=EDGE_CURVE('',#5036,#5036,#4395,.T.);
#6141=EDGE_CURVE('',#5037,#5037,#4396,.T.);
#6142=EDGE_CURVE('',#5037,#5038,#2755,.T.);
#6143=EDGE_CURVE('',#5038,#5038,#4397,.T.);
#6144=EDGE_CURVE('',#5039,#5039,#4398,.T.);
#6145=EDGE_CURVE('',#5039,#5040,#2756,.T.);
#6146=EDGE_CURVE('',#5040,#5040,#4399,.T.);
#6147=EDGE_CURVE('',#5041,#5041,#4400,.T.);
#6148=EDGE_CURVE('',#5041,#5042,#2757,.T.);
#6149=EDGE_CURVE('',#5042,#5042,#4401,.T.);
#6150=EDGE_CURVE('',#5043,#5043,#4402,.T.);
#6151=EDGE_CURVE('',#5043,#5044,#2758,.T.);
#6152=EDGE_CURVE('',#5044,#5044,#4403,.T.);
#6153=EDGE_CURVE('',#5045,#5045,#4404,.T.);
#6154=EDGE_CURVE('',#5045,#5046,#2759,.T.);
#6155=EDGE_CURVE('',#5046,#5046,#4405,.T.);
#6156=EDGE_CURVE('',#5047,#5048,#4406,.T.);
#6157=EDGE_CURVE('',#5049,#5047,#2760,.T.);
#6158=EDGE_CURVE('',#5050,#5049,#4407,.T.);
#6159=EDGE_CURVE('',#5051,#5050,#850,.F.);
#6160=EDGE_CURVE('',#5051,#5048,#2761,.T.);
#6161=EDGE_CURVE('',#5052,#5053,#4408,.T.);
#6162=EDGE_CURVE('',#5054,#5052,#4409,.T.);
#6163=EDGE_CURVE('',#5055,#5054,#4410,.T.);
#6164=EDGE_CURVE('',#5055,#5053,#4411,.T.);
#6165=EDGE_CURVE('',#5056,#5056,#4412,.T.);
#6166=EDGE_CURVE('',#5056,#5057,#4413,.T.);
#6167=EDGE_CURVE('',#5057,#5057,#4414,.T.);
#6168=EDGE_CURVE('',#5058,#5058,#4415,.T.);
#6169=EDGE_CURVE('',#5058,#5059,#4416,.T.);
#6170=EDGE_CURVE('',#5059,#5059,#4417,.T.);
#6171=EDGE_CURVE('',#5060,#5060,#4418,.T.);
#6172=EDGE_CURVE('',#5060,#5061,#4419,.T.);
#6173=EDGE_CURVE('',#5061,#5061,#4420,.T.);
#6174=EDGE_CURVE('',#5062,#5062,#4421,.T.);
#6175=EDGE_CURVE('',#5062,#5063,#4422,.T.);
#6176=EDGE_CURVE('',#5063,#5063,#4423,.T.);
#6177=EDGE_CURVE('',#5064,#5065,#4424,.T.);
#6178=EDGE_CURVE('',#5066,#5064,#4425,.T.);
#6179=EDGE_CURVE('',#5067,#5066,#4426,.T.);
#6180=EDGE_CURVE('',#5068,#5067,#4427,.T.);
#6181=EDGE_CURVE('',#5065,#5068,#4428,.T.);
#6182=EDGE_CURVE('',#5069,#5070,#4429,.T.);
#6183=EDGE_CURVE('',#5071,#5069,#4430,.T.);
#6184=EDGE_CURVE('',#5072,#5071,#4431,.T.);
#6185=EDGE_CURVE('',#5073,#5072,#4432,.T.);
#6186=EDGE_CURVE('',#5070,#5073,#4433,.T.);
#6187=EDGE_CURVE('',#5074,#5074,#4434,.T.);
#6188=EDGE_CURVE('',#5074,#5075,#4435,.T.);
#6189=EDGE_CURVE('',#5076,#5075,#4436,.T.);
#6190=EDGE_CURVE('',#5075,#5076,#4437,.T.);
#6191=EDGE_CURVE('',#5077,#5077,#4438,.T.);
#6192=EDGE_CURVE('',#5077,#5078,#4439,.T.);
#6193=EDGE_CURVE('',#5078,#5078,#4440,.T.);
#6194=EDGE_CURVE('',#5079,#5080,#4441,.T.);
#6195=EDGE_CURVE('',#5080,#5079,#4442,.T.);
#6196=EDGE_CURVE('',#5080,#5081,#4443,.T.);
#6197=EDGE_CURVE('',#5081,#5081,#4444,.T.);
#6198=EDGE_CURVE('',#5082,#5083,#4445,.T.);
#6199=EDGE_CURVE('',#5083,#5082,#4446,.T.);
#6200=EDGE_CURVE('',#5083,#5084,#4447,.T.);
#6201=EDGE_CURVE('',#5084,#5084,#4448,.T.);
#6202=EDGE_CURVE('',#5085,#5086,#4449,.T.);
#6203=EDGE_CURVE('',#5087,#5085,#2762,.T.);
#6204=EDGE_CURVE('',#5088,#5087,#4450,.T.);
#6205=EDGE_CURVE('',#5088,#5089,#747,.T.);
#6206=EDGE_CURVE('',#5090,#5089,#2763,.T.);
#6207=EDGE_CURVE('',#5086,#5090,#4451,.T.);
#6208=EDGE_CURVE('',#5091,#5092,#4452,.T.);
#6209=EDGE_CURVE('',#5091,#5093,#4453,.T.);
#6210=EDGE_CURVE('',#5094,#5093,#4454,.T.);
#6211=EDGE_CURVE('',#5092,#5094,#4455,.T.);
#6212=EDGE_CURVE('',#5095,#5095,#4456,.T.);
#6213=EDGE_CURVE('',#5095,#5096,#2764,.T.);
#6214=EDGE_CURVE('',#5096,#5096,#4457,.T.);
#6215=EDGE_CURVE('',#5061,#5039,#2765,.T.);
#6216=EDGE_CURVE('',#5067,#5035,#2766,.T.);
#6217=EDGE_CURVE('',#5066,#5068,#851,.T.);
#6218=EDGE_CURVE('',#5063,#5041,#2767,.T.);
#6219=EDGE_CURVE('',#5093,#5097,#2768,.T.);
#6220=EDGE_CURVE('',#5098,#5097,#748,.T.);
#6221=EDGE_CURVE('',#5094,#5098,#2769,.T.);
#6222=EDGE_CURVE('',#5082,#5099,#2770,.T.);
#6223=EDGE_CURVE('',#5099,#5099,#4458,.T.);
#6224=EDGE_CURVE('',#5100,#5100,#4459,.T.);
#6225=EDGE_CURVE('',#5100,#5101,#2771,.T.);
#6226=EDGE_CURVE('',#5101,#5101,#4460,.T.);
#6227=EDGE_CURVE('',#5102,#5102,#4461,.T.);
#6228=EDGE_CURVE('',#5102,#5103,#2772,.T.);
#6229=EDGE_CURVE('',#5103,#5103,#4462,.T.);
#6230=EDGE_CURVE('',#5104,#5104,#4463,.T.);
#6231=EDGE_CURVE('',#5104,#5105,#2773,.T.);
#6232=EDGE_CURVE('',#5105,#5105,#4464,.T.);
#6233=EDGE_CURVE('',#5059,#5043,#2774,.T.);
#6234=EDGE_CURVE('',#5072,#5037,#2775,.T.);
#6235=EDGE_CURVE('',#5071,#5073,#852,.T.);
#6236=EDGE_CURVE('',#5057,#5045,#2776,.T.);
#6237=EDGE_CURVE('',#5079,#5106,#2777,.T.);
#6238=EDGE_CURVE('',#5106,#5106,#4465,.T.);
#6239=EDGE_CURVE('',#5107,#5107,#4466,.T.);
#6240=EDGE_CURVE('',#5107,#5108,#2778,.T.);
#6241=EDGE_CURVE('',#5108,#5108,#4467,.T.);
#6242=EDGE_CURVE('',#5109,#5109,#4468,.T.);
#6243=EDGE_CURVE('',#5109,#5110,#2779,.T.);
#6244=EDGE_CURVE('',#5110,#5110,#4469,.T.);
#6245=EDGE_CURVE('',#5111,#5111,#4470,.T.);
#6246=EDGE_CURVE('',#5111,#5112,#2780,.T.);
#6247=EDGE_CURVE('',#5112,#5112,#4471,.T.);
#6248=EDGE_CURVE('',#5078,#5076,#2781,.T.);
#6249=EDGE_CURVE('',#5113,#5113,#4472,.T.);
#6250=EDGE_CURVE('',#5113,#5114,#2782,.T.);
#6251=EDGE_CURVE('',#5114,#5114,#4473,.T.);
#6252=EDGE_CURVE('',#5054,#5115,#2783,.T.);
#6253=EDGE_CURVE('',#5115,#5116,#749,.T.);
#6254=EDGE_CURVE('',#5055,#5116,#2784,.T.);
#6255=EDGE_CURVE('',#5117,#5117,#4474,.T.);
#6256=EDGE_CURVE('',#5117,#5118,#2785,.T.);
#6257=EDGE_CURVE('',#5118,#5118,#4475,.T.);
#6258=EDGE_CURVE('',#5119,#5120,#2786,.T.);
#6259=EDGE_CURVE('',#5119,#5121,#2787,.T.);
#6260=EDGE_CURVE('',#5121,#5122,#2788,.T.);
#6261=EDGE_CURVE('',#5122,#5123,#4476,.T.);
#6262=EDGE_CURVE('',#5120,#5123,#2789,.T.);
#6263=EDGE_CURVE('',#5124,#5125,#2790,.T.);
#6264=EDGE_CURVE('',#5125,#5126,#2791,.T.);
#6265=EDGE_CURVE('',#5127,#5126,#2792,.T.);
#6266=EDGE_CURVE('',#5127,#5124,#2793,.T.);
#6267=EDGE_CURVE('',#5090,#5128,#2794,.T.);
#6268=EDGE_CURVE('',#5128,#5129,#2795,.T.);
#6269=EDGE_CURVE('',#5130,#5129,#2796,.T.);
#6270=EDGE_CURVE('',#5086,#5130,#2797,.T.);
#6271=EDGE_CURVE('',#5131,#5132,#2798,.T.);
#6272=EDGE_CURVE('',#5131,#5133,#2799,.T.);
#6273=EDGE_CURVE('',#5133,#5134,#2800,.T.);
#6274=EDGE_CURVE('',#5134,#5135,#2801,.T.);
#6275=EDGE_CURVE('',#5135,#5132,#4477,.T.);
#6276=EDGE_CURVE('',#5136,#5137,#2802,.T.);
#6277=EDGE_CURVE('',#5137,#5138,#2803,.T.);
#6278=EDGE_CURVE('',#5139,#5138,#2804,.T.);
#6279=EDGE_CURVE('',#5139,#5136,#2805,.T.);
#6280=EDGE_CURVE('',#5140,#5141,#2806,.T.);
#6281=EDGE_CURVE('',#5141,#5142,#2807,.T.);
#6282=EDGE_CURVE('',#5143,#5142,#2808,.T.);
#6283=EDGE_CURVE('',#5143,#5144,#4478,.T.);
#6284=EDGE_CURVE('',#5144,#5140,#2809,.T.);
#6285=EDGE_CURVE('',#5145,#5146,#750,.T.);
#6286=EDGE_CURVE('',#5145,#5147,#2810,.T.);
#6287=EDGE_CURVE('',#5065,#5147,#4479,.T.);
#6288=EDGE_CURVE('',#5064,#5065,#4480,.T.);
#6289=EDGE_CURVE('',#5148,#5064,#4481,.T.);
#6290=EDGE_CURVE('',#5149,#5148,#2811,.T.);
#6291=EDGE_CURVE('',#5150,#5149,#4482,.T.);
#6292=EDGE_CURVE('',#5150,#5146,#853,.T.);
#6293=EDGE_CURVE('',#5151,#5152,#2812,.T.);
#6294=EDGE_CURVE('',#5152,#5153,#2813,.T.);
#6295=EDGE_CURVE('',#5153,#5154,#2814,.T.);
#6296=EDGE_CURVE('',#5154,#5155,#4483,.T.);
#6297=EDGE_CURVE('',#5155,#5156,#2815,.T.);
#6298=EDGE_CURVE('',#5156,#5151,#4484,.T.);
#6299=EDGE_CURVE('',#5157,#5158,#2816,.T.);
#6300=EDGE_CURVE('',#5157,#5159,#2817,.T.);
#6301=EDGE_CURVE('',#5159,#5160,#2818,.T.);
#6302=EDGE_CURVE('',#5160,#5158,#2819,.T.);
#6303=EDGE_CURVE('',#5097,#5161,#2820,.T.);
#6304=EDGE_CURVE('',#5162,#5161,#2821,.T.);
#6305=EDGE_CURVE('',#5116,#5162,#2822,.T.);
#6306=EDGE_CURVE('',#5163,#5115,#2823,.T.);
#6307=EDGE_CURVE('',#5164,#5163,#2824,.T.);
#6308=EDGE_CURVE('',#5164,#5098,#2825,.T.);
#6309=EDGE_CURVE('',#5161,#5165,#4485,.T.);
#6310=EDGE_CURVE('',#5166,#5165,#2826,.T.);
#6311=EDGE_CURVE('',#5162,#5166,#4486,.T.);
#6312=EDGE_CURVE('',#5167,#5168,#2827,.T.);
#6313=EDGE_CURVE('',#5167,#5164,#751,.T.);
#6314=EDGE_CURVE('',#5168,#5163,#752,.T.);
#6315=EDGE_CURVE('',#5165,#5169,#2828,.T.);
#6316=EDGE_CURVE('',#5169,#5170,#2829,.T.);
#6317=EDGE_CURVE('',#5166,#5170,#2830,.T.);
#6318=EDGE_CURVE('',#5171,#5168,#2831,.T.);
#6319=EDGE_CURVE('',#5171,#5172,#2832,.T.);
#6320=EDGE_CURVE('',#5172,#5167,#2833,.T.);
#6321=EDGE_CURVE('',#5173,#5120,#2834,.T.);
#6322=EDGE_CURVE('',#5173,#5055,#2835,.T.);
#6323=EDGE_CURVE('',#5170,#5119,#4487,.T.);
#6324=EDGE_CURVE('',#5054,#5174,#2836,.T.);
#6325=EDGE_CURVE('',#5174,#5130,#2837,.T.);
#6326=EDGE_CURVE('',#5129,#5171,#753,.T.);
#6327=EDGE_CURVE('',#5159,#5175,#4488,.T.);
#6328=EDGE_CURVE('',#5175,#5176,#2838,.T.);
#6329=EDGE_CURVE('',#5176,#5125,#4489,.T.);
#6330=EDGE_CURVE('',#5124,#5177,#4490,.T.);
#6331=EDGE_CURVE('',#5178,#5177,#2839,.T.);
#6332=EDGE_CURVE('',#5178,#5179,#4491,.T.);
#6333=EDGE_CURVE('',#5047,#5179,#2840,.T.);
#6334=EDGE_CURVE('',#5048,#5180,#2841,.T.);
#6335=EDGE_CURVE('',#5180,#5150,#2842,.T.);
#6336=EDGE_CURVE('',#5181,#5149,#2843,.T.);
#6337=EDGE_CURVE('',#5181,#5182,#4492,.T.);
#6338=EDGE_CURVE('',#5183,#5182,#2844,.T.);
#6339=EDGE_CURVE('',#5183,#5160,#4493,.T.);
#6340=EDGE_CURVE('',#5184,#5185,#2845,.T.);
#6341=EDGE_CURVE('',#5184,#5173,#4494,.T.);
#6342=EDGE_CURVE('',#5123,#5086,#2846,.T.);
#6343=EDGE_CURVE('',#5174,#5185,#754,.T.);
#6344=EDGE_CURVE('',#5186,#5187,#2847,.T.);
#6345=EDGE_CURVE('',#5186,#5188,#4495,.T.);
#6346=EDGE_CURVE('',#5188,#5189,#2848,.T.);
#6347=EDGE_CURVE('',#5189,#5137,#4496,.T.);
#6348=EDGE_CURVE('',#5136,#5190,#4497,.T.);
#6349=EDGE_CURVE('',#5191,#5190,#2849,.T.);
#6350=EDGE_CURVE('',#5191,#5192,#4498,.T.);
#6351=EDGE_CURVE('',#5193,#5192,#2850,.T.);
#6352=EDGE_CURVE('',#5193,#5194,#4499,.T.);
#6353=EDGE_CURVE('',#5194,#5195,#2851,.T.);
#6354=EDGE_CURVE('',#5195,#5196,#4500,.T.);
#6355=EDGE_CURVE('',#5196,#5069,#4501,.T.);
#6356=EDGE_CURVE('',#5070,#5197,#4502,.T.);
#6357=EDGE_CURVE('',#5198,#5197,#2852,.T.);
#6358=EDGE_CURVE('',#5198,#5199,#4503,.T.);
#6359=EDGE_CURVE('',#5200,#5199,#2853,.T.);
#6360=EDGE_CURVE('',#5200,#5187,#4504,.T.);
#6361=EDGE_CURVE('',#5201,#5202,#2854,.T.);
#6362=EDGE_CURVE('',#5201,#5193,#2855,.T.);
#6363=EDGE_CURVE('',#5192,#5202,#2856,.T.);
#6364=EDGE_CURVE('',#5203,#5204,#2857,.T.);
#6365=EDGE_CURVE('',#5203,#5205,#2858,.T.);
#6366=EDGE_CURVE('',#5205,#5206,#2859,.T.);
#6367=EDGE_CURVE('',#5204,#5206,#2860,.T.);
#6368=EDGE_CURVE('',#5206,#5207,#4505,.T.);
#6369=EDGE_CURVE('',#5208,#5207,#2861,.T.);
#6370=EDGE_CURVE('',#5204,#5208,#4506,.T.);
#6371=EDGE_CURVE('',#5138,#5209,#4507,.T.);
#6372=EDGE_CURVE('',#5209,#5210,#2862,.T.);
#6373=EDGE_CURVE('',#5210,#5211,#4508,.T.);
#6374=EDGE_CURVE('',#5211,#5212,#2863,.T.);
#6375=EDGE_CURVE('',#5212,#5213,#4509,.T.);
#6376=EDGE_CURVE('',#5213,#5214,#2864,.T.);
#6377=EDGE_CURVE('',#5214,#5215,#4510,.T.);
#6378=EDGE_CURVE('',#5215,#5216,#2865,.T.);
#6379=EDGE_CURVE('',#5216,#5217,#4511,.T.);
#6380=EDGE_CURVE('',#5217,#5218,#2866,.T.);
#6381=EDGE_CURVE('',#5218,#5219,#2867,.T.);
#6382=EDGE_CURVE('',#5219,#5201,#4512,.T.);
#6383=EDGE_CURVE('',#5202,#5220,#4513,.T.);
#6384=EDGE_CURVE('',#5220,#5221,#2868,.T.);
#6385=EDGE_CURVE('',#5221,#5139,#4514,.T.);
#6386=EDGE_CURVE('',#5222,#5134,#2869,.T.);
#6387=EDGE_CURVE('',#5222,#5223,#4515,.T.);
#6388=EDGE_CURVE('',#5223,#5224,#2870,.T.);
#6389=EDGE_CURVE('',#5224,#5225,#755,.T.);
#6390=EDGE_CURVE('',#5225,#5140,#2871,.T.);
#6391=EDGE_CURVE('',#5135,#5144,#2872,.T.);
#6392=EDGE_CURVE('',#5190,#5221,#2873,.T.);
#6393=EDGE_CURVE('',#5220,#5191,#2874,.T.);
#6394=EDGE_CURVE('',#5211,#5186,#2875,.T.);
#6395=EDGE_CURVE('',#5187,#5212,#2876,.T.);
#6396=EDGE_CURVE('',#5213,#5200,#2877,.T.);
#6397=EDGE_CURVE('',#5199,#5214,#2878,.T.);
#6398=EDGE_CURVE('',#5215,#5198,#2879,.T.);
#6399=EDGE_CURVE('',#5197,#5216,#2880,.T.);
#6400=EDGE_CURVE('',#5226,#5227,#2881,.T.);
#6401=EDGE_CURVE('',#5226,#5222,#2882,.T.);
#6402=EDGE_CURVE('',#5133,#5203,#4516,.T.);
#6403=EDGE_CURVE('',#5208,#5227,#2883,.T.);
#6404=EDGE_CURVE('',#5228,#5229,#2884,.T.);
#6405=EDGE_CURVE('',#5228,#5226,#4517,.T.);
#6406=EDGE_CURVE('',#5227,#5229,#756,.T.);
#6407=EDGE_CURVE('',#5225,#5228,#2885,.T.);
#6408=EDGE_CURVE('',#5229,#5230,#2886,.T.);
#6409=EDGE_CURVE('',#5230,#5231,#757,.T.);
#6410=EDGE_CURVE('',#5231,#5232,#2887,.T.);
#6411=EDGE_CURVE('',#5232,#5141,#758,.T.);
#6412=EDGE_CURVE('',#5233,#5234,#4518,.T.);
#6413=EDGE_CURVE('',#5234,#5224,#2888,.T.);
#6414=EDGE_CURVE('',#5223,#5233,#2889,.T.);
#6415=EDGE_CURVE('',#5235,#5236,#2890,.T.);
#6416=EDGE_CURVE('',#5236,#5232,#2891,.T.);
#6417=EDGE_CURVE('',#5235,#5231,#2892,.T.);
#6418=EDGE_CURVE('',#5237,#5230,#2893,.T.);
#6419=EDGE_CURVE('',#5237,#5235,#759,.T.);
#6420=EDGE_CURVE('',#5207,#5238,#2894,.T.);
#6421=EDGE_CURVE('',#5238,#5239,#760,.T.);
#6422=EDGE_CURVE('',#5239,#5237,#2895,.T.);
#6423=EDGE_CURVE('',#5240,#5241,#2896,.T.);
#6424=EDGE_CURVE('',#5241,#5242,#4519,.T.);
#6425=EDGE_CURVE('',#5242,#5243,#2897,.T.);
#6426=EDGE_CURVE('',#5243,#5240,#2898,.T.);
#6427=EDGE_CURVE('',#5205,#5131,#4520,.T.);
#6428=EDGE_CURVE('',#5132,#5244,#2899,.T.);
#6429=EDGE_CURVE('',#5244,#5245,#2900,.T.);
#6430=EDGE_CURVE('',#5245,#5238,#2901,.T.);
#6431=EDGE_CURVE('',#5245,#5246,#4521,.T.);
#6432=EDGE_CURVE('',#5246,#5239,#2902,.T.);
#6433=EDGE_CURVE('',#5142,#5236,#761,.T.);
#6434=EDGE_CURVE('',#5246,#5247,#2903,.T.);
#6435=EDGE_CURVE('',#5247,#5143,#2904,.T.);
#6436=EDGE_CURVE('',#5248,#5249,#2905,.T.);
#6437=EDGE_CURVE('',#5249,#5250,#2906,.T.);
#6438=EDGE_CURVE('',#5250,#5251,#2907,.T.);
#6439=EDGE_CURVE('',#5251,#5248,#2908,.T.);
#6440=EDGE_CURVE('',#5196,#5252,#2909,.T.);
#6441=EDGE_CURVE('',#5252,#5253,#762,.T.);
#6442=EDGE_CURVE('',#5253,#5217,#854,.T.);
#6443=EDGE_CURVE('',#5069,#5070,#4522,.T.);
#6444=EDGE_CURVE('',#5254,#5255,#2910,.T.);
#6445=EDGE_CURVE('',#5254,#5256,#2911,.T.);
#6446=EDGE_CURVE('',#5256,#5257,#2912,.T.);
#6447=EDGE_CURVE('',#5257,#5255,#2913,.T.);
#6448=EDGE_CURVE('',#5258,#5259,#2914,.T.);
#6449=EDGE_CURVE('',#5258,#5260,#2915,.T.);
#6450=EDGE_CURVE('',#5261,#5260,#2916,.T.);
#6451=EDGE_CURVE('',#5261,#5257,#4523,.T.);
#6452=EDGE_CURVE('',#5256,#5259,#4524,.T.);
#6453=EDGE_CURVE('',#5219,#5262,#2917,.T.);
#6454=EDGE_CURVE('',#5218,#5258,#763,.T.);
#6455=EDGE_CURVE('',#5259,#5262,#2918,.T.);
#6456=EDGE_CURVE('',#5263,#5264,#2919,.T.);
#6457=EDGE_CURVE('',#5264,#5265,#2920,.T.);
#6458=EDGE_CURVE('',#5265,#5266,#4525,.T.);
#6459=EDGE_CURVE('',#5263,#5266,#2921,.T.);
#6460=EDGE_CURVE('',#5267,#5263,#2922,.T.);
#6461=EDGE_CURVE('',#5267,#5261,#2923,.T.);
#6462=EDGE_CURVE('',#5260,#5253,#764,.T.);
#6463=EDGE_CURVE('',#5252,#5264,#765,.T.);
#6464=EDGE_CURVE('',#5266,#5268,#2924,.T.);
#6465=EDGE_CURVE('',#5268,#5219,#2925,.T.);
#6466=EDGE_CURVE('',#5262,#5254,#4526,.T.);
#6467=EDGE_CURVE('',#5255,#5267,#4527,.T.);
#6468=EDGE_CURVE('',#5177,#5269,#2926,.T.);
#6469=EDGE_CURVE('',#5270,#5269,#2927,.T.);
#6470=EDGE_CURVE('',#5270,#5178,#2928,.T.);
#6471=EDGE_CURVE('',#5049,#5271,#2929,.T.);
#6472=EDGE_CURVE('',#5179,#5271,#2930,.T.);
#6473=EDGE_CURVE('',#5272,#5148,#2931,.T.);
#6474=EDGE_CURVE('',#5272,#5181,#2932,.T.);
#6475=EDGE_CURVE('',#5273,#5274,#2933,.T.);
#6476=EDGE_CURVE('',#5273,#5183,#2934,.T.);
#6477=EDGE_CURVE('',#5182,#5274,#2935,.T.);
#6478=EDGE_CURVE('',#5126,#5275,#4528,.T.);
#6479=EDGE_CURVE('',#5275,#5276,#2936,.T.);
#6480=EDGE_CURVE('',#5276,#5157,#4529,.T.);
#6481=EDGE_CURVE('',#5158,#5273,#4530,.T.);
#6482=EDGE_CURVE('',#5274,#5272,#4531,.T.);
#6483=EDGE_CURVE('',#5147,#5277,#4532,.T.);
#6484=EDGE_CURVE('',#5277,#5050,#2937,.T.);
#6485=EDGE_CURVE('',#5271,#5270,#4533,.T.);
#6486=EDGE_CURVE('',#5269,#5127,#4534,.T.);
#6487=EDGE_CURVE('',#5185,#5052,#2938,.T.);
#6488=EDGE_CURVE('',#5053,#5184,#2939,.T.);
#6489=EDGE_CURVE('',#5087,#5278,#2940,.T.);
#6490=EDGE_CURVE('',#5279,#5085,#2941,.T.);
#6491=EDGE_CURVE('',#5279,#5280,#2942,.T.);
#6492=EDGE_CURVE('',#5280,#5278,#766,.T.);
#6493=EDGE_CURVE('',#5121,#5169,#4535,.T.);
#6494=EDGE_CURVE('',#5093,#5281,#2943,.T.);
#6495=EDGE_CURVE('',#5281,#5122,#2944,.T.);
#6496=EDGE_CURVE('',#5172,#5128,#767,.T.);
#6497=EDGE_CURVE('',#5089,#5094,#2945,.T.);
#6498=EDGE_CURVE('',#5092,#5088,#2946,.T.);
#6499=EDGE_CURVE('',#5278,#5091,#2947,.T.);
#6500=EDGE_CURVE('',#5282,#5283,#4536,.T.);
#6501=EDGE_CURVE('',#5283,#5284,#2948,.T.);
#6502=EDGE_CURVE('',#5285,#5284,#2949,.T.);
#6503=EDGE_CURVE('',#5285,#5282,#2950,.T.);
#6504=EDGE_CURVE('',#5151,#5286,#2951,.T.);
#6505=EDGE_CURVE('',#5286,#5285,#2952,.T.);
#6506=EDGE_CURVE('',#5284,#5145,#768,.T.);
#6507=EDGE_CURVE('',#5146,#5152,#769,.T.);
#6508=EDGE_CURVE('',#5155,#5287,#2953,.T.);
#6509=EDGE_CURVE('',#5287,#5288,#2954,.T.);
#6510=EDGE_CURVE('',#5288,#5156,#2955,.T.);
#6511=EDGE_CURVE('',#5048,#5289,#2956,.T.);
#6512=EDGE_CURVE('',#5289,#5154,#2957,.T.);
#6513=EDGE_CURVE('',#5153,#5180,#770,.T.);
#6514=EDGE_CURVE('',#5051,#5282,#2958,.T.);
#6515=EDGE_CURVE('',#5286,#5288,#4537,.T.);
#6516=EDGE_CURVE('',#5287,#5289,#4538,.T.);
#6517=EDGE_CURVE('',#5144,#5249,#4539,.T.);
#6518=EDGE_CURVE('',#5248,#5135,#4540,.T.);
#6519=EDGE_CURVE('',#5290,#5291,#2959,.T.);
#6520=EDGE_CURVE('',#5290,#5292,#2960,.T.);
#6521=EDGE_CURVE('',#5292,#5293,#2961,.T.);
#6522=EDGE_CURVE('',#5293,#5291,#2962,.T.);
#6523=EDGE_CURVE('',#5123,#5279,#4541,.T.);
#6524=EDGE_CURVE('',#5294,#5295,#2963,.T.);
#6525=EDGE_CURVE('',#5294,#5296,#2964,.T.);
#6526=EDGE_CURVE('',#5296,#5297,#2965,.T.);
#6527=EDGE_CURVE('',#5297,#5295,#2966,.T.);
#6528=EDGE_CURVE('',#5296,#5298,#4542,.T.);
#6529=EDGE_CURVE('',#5298,#5299,#2967,.T.);
#6530=EDGE_CURVE('',#5299,#5293,#4543,.T.);
#6531=EDGE_CURVE('',#5292,#5300,#4544,.T.);
#6532=EDGE_CURVE('',#5300,#5301,#2968,.T.);
#6533=EDGE_CURVE('',#5301,#5297,#4545,.T.);
#6534=EDGE_CURVE('',#5302,#5303,#2969,.T.);
#6535=EDGE_CURVE('',#5303,#5294,#4546,.T.);
#6536=EDGE_CURVE('',#5295,#5304,#4547,.T.);
#6537=EDGE_CURVE('',#5304,#5305,#2970,.T.);
#6538=EDGE_CURVE('',#5305,#5290,#4548,.T.);
#6539=EDGE_CURVE('',#5291,#5302,#4549,.T.);
#6540=EDGE_CURVE('',#5280,#5281,#771,.T.);
#6541=EDGE_CURVE('',#5244,#5251,#4550,.T.);
#6542=EDGE_CURVE('',#5250,#5247,#4551,.T.);
#6543=EDGE_CURVE('',#5251,#5243,#4552,.T.);
#6544=EDGE_CURVE('',#5240,#5250,#4553,.T.);
#6545=EDGE_CURVE('',#5244,#5243,#4554,.T.);
#6546=EDGE_CURVE('',#5240,#5247,#4555,.T.);
#6547=EDGE_CURVE('',#5245,#5242,#4556,.T.);
#6548=EDGE_CURVE('',#5241,#5246,#4557,.T.);
#6549=EDGE_CURVE('',#5277,#5283,#855,.T.);
#6550=EDGE_CURVE('',#5265,#5195,#856,.T.);
#6551=EDGE_CURVE('',#5194,#5268,#857,.T.);
#6552=EDGE_CURVE('',#5305,#5276,#858,.T.);
#6553=EDGE_CURVE('',#5275,#5300,#859,.T.);
#6554=EDGE_CURVE('',#5299,#5189,#860,.T.);
#6555=EDGE_CURVE('',#5188,#5302,#861,.T.);
#6556=EDGE_CURVE('',#5233,#5226,#4558,.T.);
#6557=EDGE_CURVE('',#5234,#5228,#4559,.T.);
#6558=EDGE_CURVE('',#5298,#5209,#862,.T.);
#6559=EDGE_CURVE('',#5176,#5301,#863,.T.);
#6560=EDGE_CURVE('',#5304,#5175,#864,.T.);
#6561=EDGE_CURVE('',#5210,#5303,#865,.T.);
#6562=EDGE_CURVE('',#5306,#5307,#4560,.T.);
#6563=EDGE_CURVE('',#5307,#5308,#2971,.T.);
#6564=EDGE_CURVE('',#5308,#5309,#4561,.T.);
#6565=EDGE_CURVE('',#5309,#5306,#2972,.T.);
#6566=EDGE_CURVE('',#5306,#5310,#2973,.T.);
#6567=EDGE_CURVE('',#5311,#5310,#4562,.T.);
#6568=EDGE_CURVE('',#5311,#5312,#2974,.T.);
#6569=EDGE_CURVE('',#5313,#5312,#2975,.T.);
#6570=EDGE_CURVE('',#5313,#5314,#4563,.T.);
#6571=EDGE_CURVE('',#5315,#5314,#2976,.T.);
#6572=EDGE_CURVE('',#5316,#5315,#2977,.T.);
#6573=EDGE_CURVE('',#5316,#5317,#4564,.T.);
#6574=EDGE_CURVE('',#5317,#5318,#2978,.T.);
#6575=EDGE_CURVE('',#5318,#5319,#4565,.T.);
#6576=EDGE_CURVE('',#5320,#5319,#2979,.T.);
#6577=EDGE_CURVE('',#5320,#5307,#4566,.T.);
#6578=EDGE_CURVE('',#5321,#5321,#4567,.T.);
#6579=EDGE_CURVE('',#5322,#5322,#4568,.T.);
#6580=EDGE_CURVE('',#5323,#5309,#2980,.T.);
#6581=EDGE_CURVE('',#5310,#5323,#2981,.T.);
#6582=EDGE_CURVE('',#5324,#5325,#4569,.T.);
#6583=EDGE_CURVE('',#5325,#5326,#2982,.T.);
#6584=EDGE_CURVE('',#5326,#5327,#4570,.T.);
#6585=EDGE_CURVE('',#5327,#5324,#2983,.T.);
#6586=EDGE_CURVE('',#5324,#5328,#2984,.T.);
#6587=EDGE_CURVE('',#5329,#5328,#4571,.T.);
#6588=EDGE_CURVE('',#5329,#5330,#2985,.T.);
#6589=EDGE_CURVE('',#5331,#5330,#2986,.T.);
#6590=EDGE_CURVE('',#5332,#5331,#4572,.T.);
#6591=EDGE_CURVE('',#5333,#5332,#2987,.T.);
#6592=EDGE_CURVE('',#5334,#5333,#2988,.T.);
#6593=EDGE_CURVE('',#5334,#5335,#4573,.T.);
#6594=EDGE_CURVE('',#5336,#5335,#2989,.T.);
#6595=EDGE_CURVE('',#5336,#5337,#2990,.T.);
#6596=EDGE_CURVE('',#5337,#5338,#2991,.T.);
#6597=EDGE_CURVE('',#5338,#5339,#4574,.T.);
#6598=EDGE_CURVE('',#5340,#5339,#2992,.T.);
#6599=EDGE_CURVE('',#5340,#5325,#4575,.T.);
#6600=EDGE_CURVE('',#5341,#5341,#4576,.T.);
#6601=EDGE_CURVE('',#5342,#5342,#4577,.T.);
#6602=EDGE_CURVE('',#5343,#5343,#4578,.T.);
#6603=EDGE_CURVE('',#5344,#5327,#2993,.T.);
#6604=EDGE_CURVE('',#5328,#5344,#2994,.T.);
#6605=EDGE_CURVE('',#5323,#5345,#4579,.T.);
#6606=EDGE_CURVE('',#5345,#5311,#2995,.T.);
#6607=EDGE_CURVE('',#5346,#5345,#2996,.T.);
#6608=EDGE_CURVE('',#5312,#5346,#2997,.T.);
#6609=EDGE_CURVE('',#5344,#5347,#4580,.T.);
#6610=EDGE_CURVE('',#5347,#5329,#2998,.T.);
#6611=EDGE_CURVE('',#5348,#5347,#2999,.T.);
#6612=EDGE_CURVE('',#5330,#5348,#3000,.T.);
#6613=EDGE_CURVE('',#5349,#5348,#3001,.T.);
#6614=EDGE_CURVE('',#5349,#5350,#866,.T.);
#6615=EDGE_CURVE('',#5350,#5331,#3002,.T.);
#6616=EDGE_CURVE('',#5326,#5351,#4581,.T.);
#6617=EDGE_CURVE('',#5351,#5352,#3003,.T.);
#6618=EDGE_CURVE('',#5352,#5353,#4582,.T.);
#6619=EDGE_CURVE('',#5353,#5354,#3004,.T.);
#6620=EDGE_CURVE('',#5354,#5355,#4583,.T.);
#6621=EDGE_CURVE('',#5355,#5356,#3005,.T.);
#6622=EDGE_CURVE('',#5356,#5357,#3006,.T.);
#6623=EDGE_CURVE('',#5357,#5349,#4584,.T.);
#6624=EDGE_CURVE('',#5358,#5358,#4585,.T.);
#6625=EDGE_CURVE('',#5359,#5359,#4586,.T.);
#6626=EDGE_CURVE('',#5346,#5360,#3007,.T.);
#6627=EDGE_CURVE('',#5360,#5361,#3008,.T.);
#6628=EDGE_CURVE('',#5361,#5313,#867,.T.);
#6629=EDGE_CURVE('',#5362,#5362,#4587,.T.);
#6630=EDGE_CURVE('',#5362,#5363,#3009,.T.);
#6631=EDGE_CURVE('',#5363,#5363,#4588,.T.);
#6632=EDGE_CURVE('',#5364,#5365,#4589,.T.);
#6633=EDGE_CURVE('',#5365,#5364,#4590,.T.);
#6634=EDGE_CURVE('',#5365,#5366,#3010,.T.);
#6635=EDGE_CURVE('',#5366,#5366,#4591,.T.);
#6636=EDGE_CURVE('',#5350,#5367,#4592,.T.);
#6637=EDGE_CURVE('',#5368,#5357,#868,.T.);
#6638=EDGE_CURVE('',#5367,#5368,#4593,.T.);
#6639=EDGE_CURVE('',#5369,#5361,#4594,.T.);
#6640=EDGE_CURVE('',#5370,#5369,#4595,.T.);
#6641=EDGE_CURVE('',#5314,#5370,#869,.T.);
#6642=EDGE_CURVE('',#5358,#5341,#3011,.T.);
#6643=EDGE_CURVE('',#5359,#5343,#3012,.T.);
#6644=EDGE_CURVE('',#5371,#5371,#4596,.T.);
#6645=EDGE_CURVE('',#5371,#5342,#3013,.T.);
#6646=EDGE_CURVE('',#5364,#5369,#3014,.T.);
#6647=EDGE_CURVE('',#5360,#5372,#4597,.T.);
#6648=EDGE_CURVE('',#5372,#5370,#3015,.T.);
#6649=EDGE_CURVE('',#5373,#5373,#4598,.T.);
#6650=EDGE_CURVE('',#5373,#5322,#3016,.T.);
#6651=EDGE_CURVE('',#5374,#5374,#4599,.T.);
#6652=EDGE_CURVE('',#5374,#5321,#3017,.T.);
#6653=EDGE_CURVE('',#5375,#5375,#4600,.T.);
#6654=EDGE_CURVE('',#5375,#5376,#3018,.T.);
#6655=EDGE_CURVE('',#5376,#5376,#4601,.T.);
#6656=EDGE_CURVE('',#5367,#5362,#3019,.T.);
#6657=EDGE_CURVE('',#5368,#5332,#3020,.T.);
#6658=EDGE_CURVE('',#5377,#5378,#3021,.T.);
#6659=EDGE_CURVE('',#5377,#5379,#3022,.T.);
#6660=EDGE_CURVE('',#5380,#5379,#3023,.T.);
#6661=EDGE_CURVE('',#5380,#5378,#3024,.T.);
#6662=EDGE_CURVE('',#5318,#5381,#870,.T.);
#6663=EDGE_CURVE('',#5382,#5381,#3025,.T.);
#6664=EDGE_CURVE('',#5382,#5353,#871,.T.);
#6665=EDGE_CURVE('',#5339,#5352,#3026,.T.);
#6666=EDGE_CURVE('',#5338,#5383,#3027,.T.);
#6667=EDGE_CURVE('',#5384,#5383,#4602,.T.);
#6668=EDGE_CURVE('',#5319,#5384,#3028,.T.);
#6669=EDGE_CURVE('',#5385,#5386,#3029,.T.);
#6670=EDGE_CURVE('',#5385,#5317,#872,.T.);
#6671=EDGE_CURVE('',#5387,#5316,#3030,.T.);
#6672=EDGE_CURVE('',#5388,#5387,#4603,.T.);
#6673=EDGE_CURVE('',#5388,#5335,#3031,.T.);
#6674=EDGE_CURVE('',#5355,#5334,#3032,.T.);
#6675=EDGE_CURVE('',#5354,#5386,#873,.T.);
#6676=EDGE_CURVE('',#5356,#5333,#3033,.T.);
#6677=EDGE_CURVE('',#5384,#5389,#3034,.T.);
#6678=EDGE_CURVE('',#5389,#5320,#3035,.T.);
#6679=EDGE_CURVE('',#5372,#5390,#3036,.T.);
#6680=EDGE_CURVE('',#5390,#5315,#3037,.T.);
#6681=EDGE_CURVE('',#5351,#5340,#3038,.T.);
#6682=EDGE_CURVE('',#5381,#5385,#3039,.T.);
#6683=EDGE_CURVE('',#5386,#5382,#3040,.T.);
#6684=EDGE_CURVE('',#5390,#5387,#3041,.T.);
#6685=EDGE_CURVE('',#5308,#5389,#4604,.T.);
#6686=EDGE_CURVE('',#5391,#5383,#3042,.T.);
#6687=EDGE_CURVE('',#5391,#5392,#3043,.T.);
#6688=EDGE_CURVE('',#5392,#5388,#3044,.T.);
#6689=EDGE_CURVE('',#5392,#5377,#4605,.T.);
#6690=EDGE_CURVE('',#5378,#5336,#4606,.T.);
#6691=EDGE_CURVE('',#5337,#5380,#4607,.T.);
#6692=EDGE_CURVE('',#5379,#5391,#4608,.T.);
#6693=EDGE_CURVE('',#5393,#5393,#4609,.T.);
#6694=EDGE_CURVE('',#5393,#5394,#3045,.T.);
#6695=EDGE_CURVE('',#5394,#5394,#4610,.T.);
#6696=EDGE_CURVE('',#5395,#5395,#4611,.T.);
#6697=EDGE_CURVE('',#5395,#5396,#3046,.T.);
#6698=EDGE_CURVE('',#5396,#5396,#4612,.T.);
#6699=EDGE_CURVE('',#5397,#5398,#4613,.T.);
#6700=EDGE_CURVE('',#5398,#5397,#4614,.T.);
#6701=EDGE_CURVE('',#5398,#5399,#3047,.T.);
#6702=EDGE_CURVE('',#5399,#5399,#4615,.T.);
#6703=EDGE_CURVE('',#5400,#5400,#4616,.T.);
#6704=EDGE_CURVE('',#5400,#5393,#3048,.T.);
#6705=EDGE_CURVE('',#5397,#5395,#3049,.T.);
#6706=EDGE_CURVE('',#5401,#5401,#4617,.T.);
#6707=EDGE_CURVE('',#5401,#5402,#3050,.T.);
#6708=EDGE_CURVE('',#5402,#5402,#4618,.T.);
#6709=EDGE_CURVE('',#5403,#5403,#4619,.T.);
#6710=EDGE_CURVE('',#5403,#5404,#3051,.T.);
#6711=EDGE_CURVE('',#5404,#5404,#4620,.T.);
#6712=EDGE_CURVE('',#5405,#5406,#4621,.T.);
#6713=EDGE_CURVE('',#5406,#5407,#3052,.T.);
#6714=EDGE_CURVE('',#5407,#5407,#4622,.T.);
#6715=EDGE_CURVE('',#5406,#5405,#4623,.T.);
#6716=EDGE_CURVE('',#5408,#5408,#4624,.T.);
#6717=EDGE_CURVE('',#5408,#5401,#3053,.T.);
#6718=EDGE_CURVE('',#5405,#5403,#3054,.T.);
#6719=EDGE_CURVE('',#5409,#5410,#4625,.T.);
#6720=EDGE_CURVE('',#5410,#5409,#4626,.T.);
#6721=EDGE_CURVE('',#5410,#5411,#3055,.T.);
#6722=EDGE_CURVE('',#5411,#5411,#4627,.T.);
#6723=EDGE_CURVE('',#5412,#5413,#4628,.T.);
#6724=EDGE_CURVE('',#5414,#5412,#19,.T.);
#6725=EDGE_CURVE('',#5415,#5414,#4629,.T.);
#6726=EDGE_CURVE('',#5413,#5415,#20,.T.);
#6727=EDGE_CURVE('',#5416,#5417,#4630,.T.);
#6728=EDGE_CURVE('',#5417,#5418,#4631,.T.);
#6729=EDGE_CURVE('',#5418,#5419,#4632,.T.);
#6730=EDGE_CURVE('',#5419,#5420,#4633,.T.);
#6731=EDGE_CURVE('',#5420,#5421,#4634,.T.);
#6732=EDGE_CURVE('',#5421,#5422,#4635,.T.);
#6733=EDGE_CURVE('',#5422,#5423,#4636,.T.);
#6734=EDGE_CURVE('',#5423,#5424,#4637,.T.);
#6735=EDGE_CURVE('',#5424,#5425,#4638,.T.);
#6736=EDGE_CURVE('',#5425,#5426,#4639,.T.);
#6737=EDGE_CURVE('',#5426,#5427,#4640,.T.);
#6738=EDGE_CURVE('',#5427,#5428,#4641,.T.);
#6739=EDGE_CURVE('',#5428,#5429,#4642,.T.);
#6740=EDGE_CURVE('',#5429,#5430,#4643,.T.);
#6741=EDGE_CURVE('',#5430,#5431,#4644,.T.);
#6742=EDGE_CURVE('',#5431,#5416,#4645,.T.);
#6743=EDGE_CURVE('',#5432,#5433,#4646,.T.);
#6744=EDGE_CURVE('',#5433,#5434,#4647,.T.);
#6745=EDGE_CURVE('',#5434,#5435,#4648,.T.);
#6746=EDGE_CURVE('',#5435,#5415,#4649,.T.);
#6747=EDGE_CURVE('',#5414,#5436,#4650,.T.);
#6748=EDGE_CURVE('',#5436,#5437,#4651,.T.);
#6749=EDGE_CURVE('',#5437,#5438,#4652,.T.);
#6750=EDGE_CURVE('',#5438,#5439,#4653,.T.);
#6751=EDGE_CURVE('',#5439,#5440,#4654,.T.);
#6752=EDGE_CURVE('',#5440,#5441,#4655,.T.);
#6753=EDGE_CURVE('',#5441,#5442,#4656,.T.);
#6754=EDGE_CURVE('',#5442,#5443,#4657,.T.);
#6755=EDGE_CURVE('',#5443,#5444,#4658,.T.);
#6756=EDGE_CURVE('',#5444,#5445,#4659,.T.);
#6757=EDGE_CURVE('',#5445,#5432,#4660,.T.);
#6758=EDGE_CURVE('',#5446,#5446,#4661,.T.);
#6759=EDGE_CURVE('',#5409,#5446,#3056,.T.);
#6760=EDGE_CURVE('',#5444,#5447,#21,.T.);
#6761=EDGE_CURVE('',#5447,#5448,#4662,.T.);
#6762=EDGE_CURVE('',#5448,#5445,#22,.T.);
#6763=EDGE_CURVE('',#5434,#5449,#23,.T.);
#6764=EDGE_CURVE('',#5449,#5450,#4663,.T.);
#6765=EDGE_CURVE('',#5450,#5435,#24,.T.);
#6766=EDGE_CURVE('',#5440,#5451,#25,.T.);
#6767=EDGE_CURVE('',#5451,#5452,#4664,.T.);
#6768=EDGE_CURVE('',#5452,#5441,#26,.T.);
#6769=EDGE_CURVE('',#5436,#5453,#27,.T.);
#6770=EDGE_CURVE('',#5453,#5454,#4665,.T.);
#6771=EDGE_CURVE('',#5454,#5437,#28,.T.);
#6772=EDGE_CURVE('',#5424,#5455,#3057,.T.);
#6773=EDGE_CURVE('',#5455,#5456,#4666,.T.);
#6774=EDGE_CURVE('',#5425,#5456,#3058,.T.);
#6775=EDGE_CURVE('',#5454,#5426,#3059,.T.);
#6776=EDGE_CURVE('',#5456,#5438,#29,.T.);
#6777=EDGE_CURVE('',#5423,#5451,#3060,.T.);
#6778=EDGE_CURVE('',#5439,#5455,#30,.T.);
#6779=EDGE_CURVE('',#5448,#5418,#3061,.T.);
#6780=EDGE_CURVE('',#5457,#5417,#3062,.T.);
#6781=EDGE_CURVE('',#5457,#5432,#31,.T.);
#6782=EDGE_CURVE('',#5431,#5449,#3063,.T.);
#6783=EDGE_CURVE('',#5433,#5458,#32,.T.);
#6784=EDGE_CURVE('',#5458,#5416,#3064,.T.);
#6785=EDGE_CURVE('',#5458,#5457,#4667,.T.);
#6786=EDGE_CURVE('',#5412,#5428,#3065,.T.);
#6787=EDGE_CURVE('',#5413,#5429,#3066,.T.);
#6788=EDGE_CURVE('',#5427,#5453,#3067,.T.);
#6789=EDGE_CURVE('',#5450,#5430,#3068,.T.);
#6790=EDGE_CURVE('',#5419,#5447,#3069,.T.);
#6791=EDGE_CURVE('',#5443,#5459,#33,.T.);
#6792=EDGE_CURVE('',#5420,#5459,#3070,.T.);
#6793=EDGE_CURVE('',#5452,#5422,#3071,.T.);
#6794=EDGE_CURVE('',#5421,#5460,#3072,.T.);
#6795=EDGE_CURVE('',#5460,#5442,#34,.T.);
#6796=EDGE_CURVE('',#5459,#5460,#4668,.T.);
#6797=EDGE_CURVE('',#5461,#5461,#4669,.T.);
#6798=EDGE_CURVE('',#5461,#5462,#3073,.T.);
#6799=EDGE_CURVE('',#5462,#5462,#4670,.T.);
#6800=EDGE_CURVE('',#5463,#5463,#4671,.T.);
#6801=EDGE_CURVE('',#5463,#5464,#4672,.T.);
#6802=EDGE_CURVE('',#5465,#5464,#4673,.T.);
#6803=EDGE_CURVE('',#5464,#5465,#4674,.T.);
#6804=EDGE_CURVE('',#5466,#5466,#4675,.T.);
#6805=EDGE_CURVE('',#5466,#5467,#4676,.T.);
#6806=EDGE_CURVE('',#5468,#5467,#4677,.T.);
#6807=EDGE_CURVE('',#5467,#5468,#4678,.T.);
#6808=EDGE_CURVE('',#5465,#5468,#3074,.T.);
#6809=EDGE_CURVE('',#5469,#5469,#4679,.T.);
#6810=EDGE_CURVE('',#5469,#5470,#3075,.T.);
#6811=EDGE_CURVE('',#5470,#5470,#4680,.T.);
#6812=EDGE_CURVE('',#5471,#5472,#874,.F.);
#6813=EDGE_CURVE('',#5472,#5473,#4681,.T.);
#6814=EDGE_CURVE('',#5473,#5474,#875,.T.);
#6815=EDGE_CURVE('',#5474,#5475,#3076,.T.);
#6816=EDGE_CURVE('',#5475,#5475,#4682,.T.);
#6817=EDGE_CURVE('',#5474,#5476,#876,.T.);
#6818=EDGE_CURVE('',#5476,#5471,#4683,.T.);
#6819=EDGE_CURVE('',#5477,#5477,#4684,.T.);
#6820=EDGE_CURVE('',#5477,#5478,#3077,.T.);
#6821=EDGE_CURVE('',#5478,#5478,#4685,.T.);
#6822=EDGE_CURVE('',#5479,#5479,#4686,.T.);
#6823=EDGE_CURVE('',#5479,#5461,#3078,.T.);
#6824=EDGE_CURVE('',#5480,#5480,#4687,.T.);
#6825=EDGE_CURVE('',#5480,#5481,#3079,.T.);
#6826=EDGE_CURVE('',#5481,#5481,#4688,.T.);
#6827=EDGE_CURVE('',#5482,#5482,#4689,.T.);
#6828=EDGE_CURVE('',#5482,#5483,#3080,.T.);
#6829=EDGE_CURVE('',#5483,#5483,#4690,.T.);
#6830=EDGE_CURVE('',#5484,#5485,#4691,.T.);
#6831=EDGE_CURVE('',#5485,#5486,#3081,.T.);
#6832=EDGE_CURVE('',#5486,#5487,#4692,.T.);
#6833=EDGE_CURVE('',#5484,#5487,#3082,.T.);
#6834=EDGE_CURVE('',#5488,#5488,#4693,.T.);
#6835=EDGE_CURVE('',#5488,#5489,#3083,.T.);
#6836=EDGE_CURVE('',#5489,#5489,#4694,.T.);
#6837=EDGE_CURVE('',#5490,#5491,#4695,.T.);
#6838=EDGE_CURVE('',#5490,#5492,#3084,.T.);
#6839=EDGE_CURVE('',#5492,#5493,#4696,.T.);
#6840=EDGE_CURVE('',#5491,#5493,#3085,.T.);
#6841=EDGE_CURVE('',#5471,#5494,#3086,.T.);
#6842=EDGE_CURVE('',#5494,#5495,#4697,.T.);
#6843=EDGE_CURVE('',#5496,#5495,#3087,.T.);
#6844=EDGE_CURVE('',#5497,#5496,#4698,.T.);
#6845=EDGE_CURVE('',#5497,#5472,#3088,.T.);
#6846=EDGE_CURVE('',#5498,#5497,#3089,.T.);
#6847=EDGE_CURVE('',#5498,#5473,#3090,.T.);
#6848=EDGE_CURVE('',#5499,#5498,#4699,.T.);
#6849=EDGE_CURVE('',#5499,#5500,#3091,.T.);
#6850=EDGE_CURVE('',#5500,#5501,#4700,.T.);
#6851=EDGE_CURVE('',#5476,#5501,#3092,.T.);
#6852=EDGE_CURVE('',#5485,#5502,#3093,.T.);
#6853=EDGE_CURVE('',#5502,#5503,#3094,.T.);
#6854=EDGE_CURVE('',#5503,#5486,#3095,.T.);
#6855=EDGE_CURVE('',#5487,#5504,#3096,.T.);
#6856=EDGE_CURVE('',#5504,#5505,#3097,.T.);
#6857=EDGE_CURVE('',#5505,#5484,#3098,.T.);
#6858=EDGE_CURVE('',#5491,#5506,#3099,.T.);
#6859=EDGE_CURVE('',#5506,#5507,#4701,.T.);
#6860=EDGE_CURVE('',#5507,#5508,#3100,.T.);
#6861=EDGE_CURVE('',#5508,#5509,#3101,.T.);
#6862=EDGE_CURVE('',#5509,#5510,#3102,.T.);
#6863=EDGE_CURVE('',#5510,#5511,#4702,.T.);
#6864=EDGE_CURVE('',#5511,#5490,#3103,.T.);
#6865=EDGE_CURVE('',#5512,#5513,#3104,.T.);
#6866=EDGE_CURVE('',#5512,#5504,#4703,.T.);
#6867=EDGE_CURVE('',#5503,#5514,#4704,.T.);
#6868=EDGE_CURVE('',#5515,#5514,#3105,.T.);
#6869=EDGE_CURVE('',#5515,#5513,#3106,.T.);
#6870=EDGE_CURVE('',#5516,#5517,#3107,.T.);
#6871=EDGE_CURVE('',#5517,#5518,#3108,.T.);
#6872=EDGE_CURVE('',#5519,#5518,#3109,.T.);
#6873=EDGE_CURVE('',#5519,#5516,#3110,.T.);
#6874=EDGE_CURVE('',#5520,#5521,#3111,.T.);
#6875=EDGE_CURVE('',#5521,#5510,#3112,.T.);
#6876=EDGE_CURVE('',#5509,#5519,#4705,.T.);
#6877=EDGE_CURVE('',#5518,#5515,#4706,.T.);
#6878=EDGE_CURVE('',#5514,#5522,#3113,.T.);
#6879=EDGE_CURVE('',#5522,#5523,#3114,.T.);
#6880=EDGE_CURVE('',#5523,#5520,#3115,.T.);
#6881=EDGE_CURVE('',#5496,#5524,#3116,.T.);
#6882=EDGE_CURVE('',#5524,#5525,#3117,.T.);
#6883=EDGE_CURVE('',#5525,#5499,#3118,.T.);
#6884=EDGE_CURVE('',#5511,#5526,#3119,.T.);
#6885=EDGE_CURVE('',#5526,#5492,#3120,.T.);
#6886=EDGE_CURVE('',#5493,#5527,#3121,.T.);
#6887=EDGE_CURVE('',#5527,#5506,#3122,.T.);
#6888=EDGE_CURVE('',#5528,#5529,#3123,.T.);
#6889=EDGE_CURVE('',#5528,#5512,#3124,.T.);
#6890=EDGE_CURVE('',#5513,#5517,#4707,.T.);
#6891=EDGE_CURVE('',#5516,#5508,#4708,.T.);
#6892=EDGE_CURVE('',#5507,#5530,#3125,.T.);
#6893=EDGE_CURVE('',#5531,#5530,#3126,.T.);
#6894=EDGE_CURVE('',#5529,#5531,#3127,.T.);
#6895=EDGE_CURVE('',#5532,#5500,#3128,.T.);
#6896=EDGE_CURVE('',#5533,#5532,#3129,.T.);
#6897=EDGE_CURVE('',#5495,#5533,#3130,.T.);
#6898=EDGE_CURVE('',#5501,#5494,#3131,.T.);
#6899=EDGE_CURVE('',#5523,#5529,#3132,.T.);
#6900=EDGE_CURVE('',#5520,#5531,#3133,.T.);
#6901=EDGE_CURVE('',#5505,#5528,#4709,.T.);
#6902=EDGE_CURVE('',#5522,#5502,#4710,.T.);
#6903=EDGE_CURVE('',#5530,#5527,#4711,.T.);
#6904=EDGE_CURVE('',#5526,#5521,#4712,.T.);
#6905=EDGE_CURVE('',#5524,#5533,#3134,.T.);
#6906=EDGE_CURVE('',#5525,#5532,#3135,.T.);
#6907=EDGE_CURVE('',#5534,#5534,#4713,.T.);
#6908=EDGE_CURVE('',#5534,#5535,#3136,.T.);
#6909=EDGE_CURVE('',#5535,#5535,#4714,.T.);
#6910=EDGE_CURVE('',#5536,#5537,#4715,.T.);
#6911=EDGE_CURVE('',#5537,#5536,#4716,.T.);
#6912=EDGE_CURVE('',#5537,#5538,#3137,.T.);
#6913=EDGE_CURVE('',#5538,#5538,#4717,.T.);
#6914=EDGE_CURVE('',#5536,#5534,#3138,.T.);
#6915=EDGE_CURVE('',#5539,#5539,#4718,.T.);
#6916=EDGE_CURVE('',#5539,#5540,#3139,.T.);
#6917=EDGE_CURVE('',#5540,#5540,#4719,.T.);
#6918=EDGE_CURVE('',#5541,#5542,#4720,.T.);
#6919=EDGE_CURVE('',#5542,#5541,#4721,.T.);
#6920=EDGE_CURVE('',#5542,#5543,#3140,.T.);
#6921=EDGE_CURVE('',#5543,#5543,#4722,.T.);
#6922=EDGE_CURVE('',#5541,#5539,#3141,.T.);
#6923=EDGE_CURVE('',#5544,#5544,#4723,.T.);
#6924=EDGE_CURVE('',#5544,#5545,#3142,.T.);
#6925=EDGE_CURVE('',#5545,#5545,#4724,.T.);
#6926=EDGE_CURVE('',#5546,#5546,#4725,.T.);
#6927=EDGE_CURVE('',#5546,#5547,#3143,.T.);
#6928=EDGE_CURVE('',#5547,#5547,#4726,.T.);
#6929=EDGE_CURVE('',#5548,#5549,#3144,.T.);
#6930=EDGE_CURVE('',#5549,#5550,#4727,.T.);
#6931=EDGE_CURVE('',#5550,#5551,#3145,.T.);
#6932=EDGE_CURVE('',#5551,#5552,#4728,.T.);
#6933=EDGE_CURVE('',#5552,#5553,#3146,.T.);
#6934=EDGE_CURVE('',#5553,#5554,#4729,.T.);
#6935=EDGE_CURVE('',#5554,#5555,#3147,.T.);
#6936=EDGE_CURVE('',#5555,#5548,#4730,.T.);
#6937=EDGE_CURVE('',#5556,#5557,#3148,.T.);
#6938=EDGE_CURVE('',#5556,#5558,#4731,.T.);
#6939=EDGE_CURVE('',#5559,#5558,#3149,.T.);
#6940=EDGE_CURVE('',#5559,#5560,#4732,.T.);
#6941=EDGE_CURVE('',#5561,#5560,#3150,.T.);
#6942=EDGE_CURVE('',#5561,#5562,#4733,.T.);
#6943=EDGE_CURVE('',#5563,#5562,#3151,.T.);
#6944=EDGE_CURVE('',#5563,#5557,#4734,.T.);
#6945=EDGE_CURVE('',#5550,#5556,#3152,.T.);
#6946=EDGE_CURVE('',#5557,#5551,#3153,.T.);
#6947=EDGE_CURVE('',#5552,#5563,#3154,.T.);
#6948=EDGE_CURVE('',#5562,#5553,#3155,.T.);
#6949=EDGE_CURVE('',#5560,#5555,#3156,.T.);
#6950=EDGE_CURVE('',#5554,#5561,#3157,.T.);
#6951=EDGE_CURVE('',#5558,#5549,#3158,.T.);
#6952=EDGE_CURVE('',#5548,#5559,#3159,.T.);
#6953=EDGE_CURVE('',#5564,#5565,#877,.T.);
#6954=EDGE_CURVE('',#5565,#5566,#3160,.T.);
#6955=EDGE_CURVE('',#5566,#5566,#4735,.T.);
#6956=EDGE_CURVE('',#5565,#5564,#878,.T.);
#6957=EDGE_CURVE('',#5567,#5567,#4736,.T.);
#6958=EDGE_CURVE('',#5567,#5568,#4737,.T.);
#6959=EDGE_CURVE('',#5569,#5568,#4738,.T.);
#6960=EDGE_CURVE('',#5568,#5569,#4739,.T.);
#6961=EDGE_CURVE('',#5570,#5571,#4740,.T.);
#6962=EDGE_CURVE('',#5571,#5570,#4741,.T.);
#6963=EDGE_CURVE('',#5571,#5572,#4742,.T.);
#6964=EDGE_CURVE('',#5572,#5572,#4743,.T.);
#6965=EDGE_CURVE('',#5573,#5573,#4744,.T.);
#6966=EDGE_CURVE('',#5573,#5574,#3161,.T.);
#6967=EDGE_CURVE('',#5574,#5574,#4745,.T.);
#6968=EDGE_CURVE('',#5575,#5575,#4746,.T.);
#6969=EDGE_CURVE('',#5575,#5576,#3162,.T.);
#6970=EDGE_CURVE('',#5576,#5576,#4747,.T.);
#6971=EDGE_CURVE('',#5577,#5577,#4748,.T.);
#6972=EDGE_CURVE('',#5577,#5578,#3163,.T.);
#6973=EDGE_CURVE('',#5578,#5578,#4749,.T.);
#6974=EDGE_CURVE('',#5579,#5579,#4750,.T.);
#6975=EDGE_CURVE('',#5579,#5580,#3164,.T.);
#6976=EDGE_CURVE('',#5580,#5580,#4751,.T.);
#6977=EDGE_CURVE('',#5581,#5582,#772,.T.);
#6978=EDGE_CURVE('',#5583,#5581,#773,.T.);
#6979=EDGE_CURVE('',#5584,#5583,#3165,.T.);
#6980=EDGE_CURVE('',#5585,#5584,#774,.T.);
#6981=EDGE_CURVE('',#5586,#5585,#775,.T.);
#6982=EDGE_CURVE('',#5587,#5586,#3166,.T.);
#6983=EDGE_CURVE('',#5587,#5582,#776,.T.);
#6984=EDGE_CURVE('',#5588,#5589,#777,.T.);
#6985=EDGE_CURVE('',#5590,#5588,#778,.T.);
#6986=EDGE_CURVE('',#5591,#5590,#3167,.T.);
#6987=EDGE_CURVE('',#5592,#5591,#779,.T.);
#6988=EDGE_CURVE('',#5593,#5592,#780,.T.);
#6989=EDGE_CURVE('',#5593,#5594,#781,.T.);
#6990=EDGE_CURVE('',#5589,#5594,#3168,.T.);
#6991=EDGE_CURVE('',#5595,#5595,#4752,.T.);
#6992=EDGE_CURVE('',#5595,#5596,#3169,.T.);
#6993=EDGE_CURVE('',#5597,#5596,#4753,.T.);
#6994=EDGE_CURVE('',#5598,#5597,#4754,.T.);
#6995=EDGE_CURVE('',#5599,#5598,#4755,.T.);
#6996=EDGE_CURVE('',#5600,#5599,#4756,.T.);
#6997=EDGE_CURVE('',#5601,#5600,#4757,.T.);
#6998=EDGE_CURVE('',#5596,#5601,#4758,.T.);
#6999=EDGE_CURVE('',#5602,#5603,#4759,.T.);
#7000=EDGE_CURVE('',#5604,#5602,#3170,.T.);
#7001=EDGE_CURVE('',#5605,#5604,#4760,.T.);
#7002=EDGE_CURVE('',#5603,#5605,#3171,.T.);
#7003=EDGE_CURVE('',#5606,#5606,#4761,.T.);
#7004=EDGE_CURVE('',#5606,#5607,#3172,.T.);
#7005=EDGE_CURVE('',#5607,#5607,#4762,.T.);
#7006=EDGE_CURVE('',#5608,#5608,#4763,.T.);
#7007=EDGE_CURVE('',#5608,#5609,#3173,.T.);
#7008=EDGE_CURVE('',#5609,#5609,#4764,.T.);
#7009=EDGE_CURVE('',#5610,#5610,#4765,.T.);
#7010=EDGE_CURVE('',#5610,#5611,#3174,.T.);
#7011=EDGE_CURVE('',#5611,#5611,#4766,.T.);
#7012=EDGE_CURVE('',#5612,#5612,#4767,.T.);
#7013=EDGE_CURVE('',#5612,#5613,#3175,.T.);
#7014=EDGE_CURVE('',#5613,#5614,#4768,.T.);
#7015=EDGE_CURVE('',#5614,#5615,#4769,.T.);
#7016=EDGE_CURVE('',#5615,#5613,#4770,.T.);
#7017=EDGE_CURVE('',#5616,#5617,#782,.F.);
#7018=EDGE_CURVE('',#5617,#5614,#35,.T.);
#7019=EDGE_CURVE('',#5613,#5618,#3176,.T.);
#7020=EDGE_CURVE('',#5618,#5619,#4771,.T.);
#7021=EDGE_CURVE('',#5619,#5620,#4772,.T.);
#7022=EDGE_CURVE('',#5620,#5621,#4773,.T.);
#7023=EDGE_CURVE('',#5621,#5622,#4774,.T.);
#7024=EDGE_CURVE('',#5622,#5618,#4775,.T.);
#7025=EDGE_CURVE('',#5615,#5616,#879,.T.);
#7026=EDGE_CURVE('',#5570,#5623,#3177,.T.);
#7027=EDGE_CURVE('',#5623,#5624,#880,.T.);
#7028=EDGE_CURVE('',#5624,#5625,#881,.T.);
#7029=EDGE_CURVE('',#5625,#5626,#3178,.T.);
#7030=EDGE_CURVE('',#5626,#5627,#882,.T.);
#7031=EDGE_CURVE('',#5627,#5628,#883,.T.);
#7032=EDGE_CURVE('',#5628,#5569,#3179,.T.);
#7033=EDGE_CURVE('',#5628,#5629,#884,.T.);
#7034=EDGE_CURVE('',#5630,#5629,#885,.T.);
#7035=EDGE_CURVE('',#5630,#5631,#3180,.T.);
#7036=EDGE_CURVE('',#5632,#5631,#886,.T.);
#7037=EDGE_CURVE('',#5632,#5623,#887,.T.);
#7038=EDGE_CURVE('',#5633,#5634,#3181,.T.);
#7039=EDGE_CURVE('',#5634,#5635,#3182,.T.);
#7040=EDGE_CURVE('',#5635,#5636,#3183,.T.);
#7041=EDGE_CURVE('',#5636,#5633,#3184,.T.);
#7042=EDGE_CURVE('',#5637,#5638,#3185,.T.);
#7043=EDGE_CURVE('',#5638,#5626,#888,.T.);
#7044=EDGE_CURVE('',#5625,#5637,#889,.T.);
#7045=EDGE_CURVE('',#5639,#5640,#3186,.T.);
#7046=EDGE_CURVE('',#5640,#5638,#3187,.T.);
#7047=EDGE_CURVE('',#5637,#5639,#3188,.T.);
#7048=EDGE_CURVE('',#5622,#5640,#4776,.T.);
#7049=EDGE_CURVE('',#5639,#5619,#4777,.T.);
#7050=EDGE_CURVE('',#5633,#5621,#4778,.T.);
#7051=EDGE_CURVE('',#5620,#5634,#4779,.T.);
#7052=EDGE_CURVE('',#5641,#5642,#3189,.T.);
#7053=EDGE_CURVE('',#5643,#5641,#3190,.T.);
#7054=EDGE_CURVE('',#5644,#5643,#3191,.T.);
#7055=EDGE_CURVE('',#5645,#5644,#3192,.T.);
#7056=EDGE_CURVE('',#5646,#5645,#3193,.T.);
#7057=EDGE_CURVE('',#5642,#5646,#3194,.T.);
#7058=EDGE_CURVE('',#5647,#5642,#3195,.T.);
#7059=EDGE_CURVE('',#5647,#5648,#3196,.T.);
#7060=EDGE_CURVE('',#5648,#5641,#3197,.T.);
#7061=EDGE_CURVE('',#5649,#5646,#3198,.T.);
#7062=EDGE_CURVE('',#5649,#5647,#3199,.T.);
#7063=EDGE_CURVE('',#5650,#5645,#3200,.T.);
#7064=EDGE_CURVE('',#5650,#5649,#3201,.T.);
#7065=EDGE_CURVE('',#5651,#5644,#3202,.T.);
#7066=EDGE_CURVE('',#5651,#5650,#3203,.T.);
#7067=EDGE_CURVE('',#5652,#5643,#3204,.T.);
#7068=EDGE_CURVE('',#5652,#5651,#3205,.T.);
#7069=EDGE_CURVE('',#5648,#5652,#3206,.T.);
#7070=EDGE_CURVE('',#5653,#5654,#3207,.T.);
#7071=EDGE_CURVE('',#5654,#5655,#3208,.T.);
#7072=EDGE_CURVE('',#5655,#5656,#3209,.T.);
#7073=EDGE_CURVE('',#5656,#5657,#3210,.T.);
#7074=EDGE_CURVE('',#5657,#5658,#3211,.T.);
#7075=EDGE_CURVE('',#5658,#5653,#3212,.T.);
#7076=EDGE_CURVE('',#5659,#5660,#3213,.T.);
#7077=EDGE_CURVE('',#5661,#5659,#3214,.T.);
#7078=EDGE_CURVE('',#5662,#5661,#3215,.T.);
#7079=EDGE_CURVE('',#5662,#5663,#3216,.T.);
#7080=EDGE_CURVE('',#5663,#5604,#3217,.T.);
#7081=EDGE_CURVE('',#5602,#5664,#3218,.T.);
#7082=EDGE_CURVE('',#5664,#5660,#3219,.T.);
#7083=EDGE_CURVE('',#5614,#5663,#3220,.T.);
#7084=EDGE_CURVE('',#5665,#5662,#3221,.T.);
#7085=EDGE_CURVE('',#5666,#5665,#3222,.T.);
#7086=EDGE_CURVE('',#5666,#5660,#3223,.T.);
#7087=EDGE_CURVE('',#5615,#5664,#3224,.T.);
#7088=EDGE_CURVE('',#5616,#5603,#3225,.T.);
#7089=EDGE_CURVE('',#5617,#5605,#3226,.T.);
#7090=EDGE_CURVE('',#5667,#5661,#3227,.T.);
#7091=EDGE_CURVE('',#5667,#5668,#4780,.T.);
#7092=EDGE_CURVE('',#5665,#5668,#3228,.T.);
#7093=EDGE_CURVE('',#5669,#5659,#3229,.T.);
#7094=EDGE_CURVE('',#5669,#5667,#3230,.T.);
#7095=EDGE_CURVE('',#5670,#5666,#3231,.T.);
#7096=EDGE_CURVE('',#5670,#5669,#4781,.T.);
#7097=EDGE_CURVE('',#5668,#5670,#3232,.T.);
#7098=EDGE_CURVE('',#5596,#5671,#3233,.T.);
#7099=EDGE_CURVE('',#5671,#5601,#3234,.T.);
#7100=EDGE_CURVE('',#5601,#5672,#3235,.T.);
#7101=EDGE_CURVE('',#5672,#5600,#3236,.T.);
#7102=EDGE_CURVE('',#5600,#5673,#3237,.T.);
#7103=EDGE_CURVE('',#5673,#5599,#3238,.T.);
#7104=EDGE_CURVE('',#5599,#5674,#3239,.T.);
#7105=EDGE_CURVE('',#5674,#5598,#3240,.T.);
#7106=EDGE_CURVE('',#5598,#5675,#3241,.T.);
#7107=EDGE_CURVE('',#5675,#5597,#3242,.T.);
#7108=EDGE_CURVE('',#5597,#5676,#3243,.T.);
#7109=EDGE_CURVE('',#5676,#5596,#3244,.T.);
#7110=EDGE_CURVE('',#5584,#5677,#3245,.T.);
#7111=EDGE_CURVE('',#5677,#5678,#783,.T.);
#7112=EDGE_CURVE('',#5678,#5674,#3246,.T.);
#7113=EDGE_CURVE('',#5585,#5675,#3247,.T.);
#7114=EDGE_CURVE('',#5679,#5586,#3248,.T.);
#7115=EDGE_CURVE('',#5680,#5676,#3249,.T.);
#7116=EDGE_CURVE('',#5680,#5679,#784,.T.);
#7117=EDGE_CURVE('',#5681,#5682,#3250,.T.);
#7118=EDGE_CURVE('',#5682,#5680,#785,.T.);
#7119=EDGE_CURVE('',#5683,#5671,#3251,.T.);
#7120=EDGE_CURVE('',#5683,#5681,#786,.T.);
#7121=EDGE_CURVE('',#5589,#5684,#3252,.T.);
#7122=EDGE_CURVE('',#5684,#5683,#787,.T.);
#7123=EDGE_CURVE('',#5588,#5672,#3253,.T.);
#7124=EDGE_CURVE('',#5685,#5673,#3254,.T.);
#7125=EDGE_CURVE('',#5685,#5686,#788,.T.);
#7126=EDGE_CURVE('',#5686,#5590,#3255,.T.);
#7127=EDGE_CURVE('',#5678,#5687,#789,.T.);
#7128=EDGE_CURVE('',#5687,#5688,#3256,.T.);
#7129=EDGE_CURVE('',#5688,#5685,#790,.T.);
#7130=EDGE_CURVE('',#5592,#5689,#791,.T.);
#7131=EDGE_CURVE('',#5689,#5581,#792,.T.);
#7132=EDGE_CURVE('',#5582,#5690,#793,.T.);
#7133=EDGE_CURVE('',#5690,#5593,#794,.T.);
#7134=EDGE_CURVE('',#5583,#5677,#3257,.T.);
#7135=EDGE_CURVE('',#5679,#5587,#3258,.T.);
#7136=EDGE_CURVE('',#5687,#5691,#3259,.T.);
#7137=EDGE_CURVE('',#5691,#5688,#3260,.T.);
#7138=EDGE_CURVE('',#5681,#5692,#3261,.T.);
#7139=EDGE_CURVE('',#5692,#5682,#3262,.T.);
#7140=EDGE_CURVE('',#5686,#5591,#3263,.T.);
#7141=EDGE_CURVE('',#5594,#5684,#3264,.T.);
#7142=EDGE_CURVE('',#5692,#5690,#795,.T.);
#7143=EDGE_CURVE('',#5689,#5691,#796,.T.);
#7144=EDGE_CURVE('',#5693,#5694,#890,.T.);
#7145=EDGE_CURVE('',#5694,#5622,#3265,.T.);
#7146=EDGE_CURVE('',#5621,#5695,#3266,.T.);
#7147=EDGE_CURVE('',#5695,#5693,#891,.T.);
#7148=EDGE_CURVE('',#5619,#5696,#3267,.T.);
#7149=EDGE_CURVE('',#5696,#5697,#892,.T.);
#7150=EDGE_CURVE('',#5697,#5698,#893,.T.);
#7151=EDGE_CURVE('',#5698,#5620,#3268,.T.);
#7152=EDGE_CURVE('',#5696,#5637,#4782,.T.);
#7153=EDGE_CURVE('',#5697,#5625,#894,.T.);
#7154=EDGE_CURVE('',#5697,#5624,#4783,.T.);
#7155=EDGE_CURVE('',#5698,#5632,#4784,.T.);
#7156=EDGE_CURVE('',#5635,#5698,#895,.T.);
#7157=EDGE_CURVE('',#5635,#5631,#4785,.T.);
#7158=EDGE_CURVE('',#5638,#5694,#4786,.T.);
#7159=EDGE_CURVE('',#5636,#5630,#4787,.T.);
#7160=EDGE_CURVE('',#5695,#5636,#896,.T.);
#7161=EDGE_CURVE('',#5626,#5693,#897,.T.);
#7162=EDGE_CURVE('',#5695,#5629,#4788,.T.);
#7163=EDGE_CURVE('',#5627,#5693,#4789,.T.);
#7164=EDGE_CURVE('',#5649,#5657,#797,.T.);
#7165=EDGE_CURVE('',#5658,#5650,#798,.T.);
#7166=EDGE_CURVE('',#5653,#5651,#799,.T.);
#7167=EDGE_CURVE('',#5647,#5656,#800,.T.);
#7168=EDGE_CURVE('',#5654,#5652,#801,.T.);
#7169=EDGE_CURVE('',#5648,#5655,#802,.T.);
#7170=EDGE_CURVE('',#5699,#5700,#4790,.T.);
#7171=EDGE_CURVE('',#5701,#5699,#898,.F.);
#7172=EDGE_CURVE('',#5702,#5701,#4791,.T.);
#7173=EDGE_CURVE('',#5702,#5703,#3269,.T.);
#7174=EDGE_CURVE('',#5703,#5703,#4792,.T.);
#7175=EDGE_CURVE('',#5704,#5702,#4793,.T.);
#7176=EDGE_CURVE('',#5700,#5704,#899,.F.);
#7177=EDGE_CURVE('',#5705,#5704,#900,.F.);
#7178=EDGE_CURVE('',#5705,#5706,#3270,.T.);
#7179=EDGE_CURVE('',#5706,#5706,#4794,.T.);
#7180=EDGE_CURVE('',#5700,#5705,#901,.F.);
#7181=EDGE_CURVE('',#5707,#5707,#4795,.T.);
#7182=EDGE_CURVE('',#5707,#5708,#3271,.T.);
#7183=EDGE_CURVE('',#5701,#5708,#902,.F.);
#7184=EDGE_CURVE('',#5708,#5699,#903,.F.);
#7185=EDGE_CURVE('',#5709,#5710,#4796,.T.);
#7186=EDGE_CURVE('',#5710,#5711,#3272,.T.);
#7187=EDGE_CURVE('',#5711,#5712,#4797,.T.);
#7188=EDGE_CURVE('',#5712,#5711,#4798,.T.);
#7189=EDGE_CURVE('',#5710,#5709,#4799,.T.);
#7190=EDGE_CURVE('',#5713,#5713,#4800,.T.);
#7191=EDGE_CURVE('',#5713,#5712,#3273,.T.);
#7192=EDGE_CURVE('',#5709,#5702,#3274,.T.);
#7193=EDGE_CURVE('',#5714,#5714,#4801,.T.);
#7194=EDGE_CURVE('',#5714,#5715,#3275,.T.);
#7195=EDGE_CURVE('',#5715,#5715,#4802,.T.);
#7196=EDGE_CURVE('',#5716,#5716,#4803,.T.);
#7197=EDGE_CURVE('',#5716,#5717,#3276,.T.);
#7198=EDGE_CURVE('',#5717,#5717,#4804,.T.);
#7199=EDGE_CURVE('',#5718,#5718,#4805,.T.);
#7200=EDGE_CURVE('',#5718,#5719,#3277,.T.);
#7201=EDGE_CURVE('',#5719,#5719,#4806,.T.);
#7202=EDGE_CURVE('',#5720,#5720,#4807,.T.);
#7203=EDGE_CURVE('',#5720,#5721,#3278,.T.);
#7204=EDGE_CURVE('',#5721,#5721,#4808,.T.);
#7205=EDGE_CURVE('',#5722,#5722,#4809,.T.);
#7206=EDGE_CURVE('',#5722,#5723,#3279,.T.);
#7207=EDGE_CURVE('',#5723,#5723,#4810,.T.);
#7208=EDGE_CURVE('',#5724,#5724,#4811,.T.);
#7209=EDGE_CURVE('',#5724,#5724,#4812,.T.);
#7210=EDGE_CURVE('',#5725,#5726,#3280,.T.);
#7211=EDGE_CURVE('',#5725,#5727,#3281,.T.);
#7212=EDGE_CURVE('',#5727,#5728,#3282,.T.);
#7213=EDGE_CURVE('',#5729,#5728,#3283,.T.);
#7214=EDGE_CURVE('',#5730,#5729,#3284,.T.);
#7215=EDGE_CURVE('',#5730,#5731,#3285,.T.);
#7216=EDGE_CURVE('',#5732,#5731,#3286,.T.);
#7217=EDGE_CURVE('',#5726,#5732,#4813,.T.);
#7218=EDGE_CURVE('',#5733,#5734,#3287,.T.);
#7219=EDGE_CURVE('',#5733,#5735,#3288,.T.);
#7220=EDGE_CURVE('',#5736,#5735,#3289,.T.);
#7221=EDGE_CURVE('',#5737,#5736,#4814,.T.);
#7222=EDGE_CURVE('',#5738,#5737,#3290,.T.);
#7223=EDGE_CURVE('',#5738,#5739,#3291,.T.);
#7224=EDGE_CURVE('',#5739,#5740,#3292,.T.);
#7225=EDGE_CURVE('',#5740,#5734,#3293,.T.);
#7226=EDGE_CURVE('',#5739,#5730,#3294,.T.);
#7227=EDGE_CURVE('',#5729,#5741,#4815,.T.);
#7228=EDGE_CURVE('',#5741,#5742,#3295,.T.);
#7229=EDGE_CURVE('',#5742,#5743,#4816,.T.);
#7230=EDGE_CURVE('',#5743,#5744,#3296,.T.);
#7231=EDGE_CURVE('',#5744,#5745,#4817,.T.);
#7232=EDGE_CURVE('',#5745,#5746,#3297,.T.);
#7233=EDGE_CURVE('',#5746,#5747,#4818,.T.);
#7234=EDGE_CURVE('',#5747,#5748,#3298,.T.);
#7235=EDGE_CURVE('',#5748,#5749,#3299,.T.);
#7236=EDGE_CURVE('',#5750,#5749,#3300,.T.);
#7237=EDGE_CURVE('',#5751,#5750,#4819,.T.);
#7238=EDGE_CURVE('',#5752,#5751,#3301,.T.);
#7239=EDGE_CURVE('',#5753,#5752,#4820,.T.);
#7240=EDGE_CURVE('',#5754,#5753,#3302,.T.);
#7241=EDGE_CURVE('',#5755,#5754,#4821,.T.);
#7242=EDGE_CURVE('',#5756,#5755,#3303,.T.);
#7243=EDGE_CURVE('',#5740,#5756,#4822,.T.);
#7244=EDGE_CURVE('',#5757,#5758,#3304,.T.);
#7245=EDGE_CURVE('',#5758,#5759,#3305,.T.);
#7246=EDGE_CURVE('',#5760,#5759,#3306,.T.);
#7247=EDGE_CURVE('',#5761,#5760,#4823,.T.);
#7248=EDGE_CURVE('',#5762,#5761,#3307,.T.);
#7249=EDGE_CURVE('',#5763,#5762,#4824,.T.);
#7250=EDGE_CURVE('',#5764,#5763,#3308,.T.);
#7251=EDGE_CURVE('',#5765,#5764,#4825,.T.);
#7252=EDGE_CURVE('',#5766,#5765,#3309,.T.);
#7253=EDGE_CURVE('',#5728,#5766,#4826,.T.);
#7254=EDGE_CURVE('',#5727,#5733,#3310,.T.);
#7255=EDGE_CURVE('',#5734,#5767,#4827,.T.);
#7256=EDGE_CURVE('',#5767,#5768,#3311,.T.);
#7257=EDGE_CURVE('',#5768,#5769,#4828,.T.);
#7258=EDGE_CURVE('',#5769,#5770,#3312,.T.);
#7259=EDGE_CURVE('',#5770,#5771,#4829,.T.);
#7260=EDGE_CURVE('',#5771,#5772,#3313,.T.);
#7261=EDGE_CURVE('',#5772,#5757,#4830,.T.);
#7262=EDGE_CURVE('',#5741,#5766,#3314,.T.);
#7263=EDGE_CURVE('',#5742,#5765,#3315,.T.);
#7264=EDGE_CURVE('',#5743,#5764,#3316,.T.);
#7265=EDGE_CURVE('',#5744,#5763,#3317,.T.);
#7266=EDGE_CURVE('',#5745,#5762,#3318,.T.);
#7267=EDGE_CURVE('',#5746,#5761,#3319,.T.);
#7268=EDGE_CURVE('',#5747,#5760,#3320,.T.);
#7269=EDGE_CURVE('',#5759,#5773,#3321,.T.);
#7270=EDGE_CURVE('',#5774,#5773,#3322,.T.);
#7271=EDGE_CURVE('',#5775,#5774,#4831,.T.);
#7272=EDGE_CURVE('',#5776,#5775,#3323,.T.);
#7273=EDGE_CURVE('',#5776,#5748,#3324,.T.);
#7274=EDGE_CURVE('',#5756,#5767,#3325,.T.);
#7275=EDGE_CURVE('',#5755,#5768,#3326,.T.);
#7276=EDGE_CURVE('',#5754,#5769,#3327,.T.);
#7277=EDGE_CURVE('',#5753,#5770,#3328,.T.);
#7278=EDGE_CURVE('',#5752,#5771,#3329,.T.);
#7279=EDGE_CURVE('',#5751,#5772,#3330,.T.);
#7280=EDGE_CURVE('',#5750,#5757,#3331,.T.);
#7281=EDGE_CURVE('',#5777,#5778,#3332,.T.);
#7282=EDGE_CURVE('',#5777,#5758,#3333,.T.);
#7283=EDGE_CURVE('',#5749,#5779,#3334,.T.);
#7284=EDGE_CURVE('',#5780,#5779,#3335,.T.);
#7285=EDGE_CURVE('',#5778,#5780,#4832,.T.);
#7286=EDGE_CURVE('',#5779,#5776,#3336,.T.);
#7287=EDGE_CURVE('',#5780,#5775,#3337,.T.);
#7288=EDGE_CURVE('',#5778,#5774,#3338,.T.);
#7289=EDGE_CURVE('',#5773,#5777,#3339,.T.);
#7290=EDGE_CURVE('',#5731,#5738,#3340,.T.);
#7291=EDGE_CURVE('',#5737,#5732,#3341,.T.);
#7292=EDGE_CURVE('',#5736,#5726,#3342,.T.);
#7293=EDGE_CURVE('',#5735,#5725,#3343,.T.);
#7294=EDGE_CURVE('',#5781,#5782,#904,.T.);
#7295=EDGE_CURVE('',#5781,#5783,#3344,.T.);
#7296=EDGE_CURVE('',#5784,#5783,#905,.T.);
#7297=EDGE_CURVE('',#5782,#5784,#3345,.T.);
#7298=EDGE_CURVE('',#5785,#5786,#906,.T.);
#7299=EDGE_CURVE('',#5785,#5787,#3346,.T.);
#7300=EDGE_CURVE('',#5788,#5787,#907,.T.);
#7301=EDGE_CURVE('',#5786,#5788,#3347,.T.);
#7302=EDGE_CURVE('',#5782,#5781,#908,.T.);
#7303=EDGE_CURVE('',#5781,#5785,#3348,.T.);
#7304=EDGE_CURVE('',#5786,#5785,#909,.T.);
#7305=EDGE_CURVE('',#5784,#5788,#4833,.T.);
#7306=EDGE_CURVE('',#5784,#5789,#3349,.T.);
#7307=EDGE_CURVE('',#5789,#5789,#4834,.T.);
#7308=EDGE_CURVE('',#5788,#5784,#4835,.T.);
#7309=EDGE_CURVE('',#5790,#5790,#4836,.T.);
#7310=EDGE_CURVE('',#5790,#5783,#3350,.T.);
#7311=EDGE_CURVE('',#5783,#5784,#910,.T.);
#7312=EDGE_CURVE('',#5787,#5788,#911,.T.);
#7313=EDGE_CURVE('',#5791,#5791,#4837,.T.);
#7314=EDGE_CURVE('',#5791,#5790,#4838,.T.);
#7315=EDGE_CURVE('',#5792,#5793,#4839,.T.);
#7316=EDGE_CURVE('',#5793,#5792,#4840,.T.);
#7317=EDGE_CURVE('',#5793,#5794,#3351,.T.);
#7318=EDGE_CURVE('',#5794,#5794,#4841,.T.);
#7319=EDGE_CURVE('',#5792,#5795,#3352,.T.);
#7320=EDGE_CURVE('',#5795,#5795,#4842,.T.);
#7321=EDGE_CURVE('',#5796,#5797,#912,.T.);
#7322=EDGE_CURVE('',#5796,#5798,#3353,.T.);
#7323=EDGE_CURVE('',#5799,#5798,#913,.T.);
#7324=EDGE_CURVE('',#5797,#5799,#3354,.T.);
#7325=EDGE_CURVE('',#5800,#5801,#914,.T.);
#7326=EDGE_CURVE('',#5800,#5802,#3355,.T.);
#7327=EDGE_CURVE('',#5803,#5802,#915,.T.);
#7328=EDGE_CURVE('',#5801,#5803,#3356,.T.);
#7329=EDGE_CURVE('',#5797,#5796,#916,.T.);
#7330=EDGE_CURVE('',#5796,#5800,#3357,.T.);
#7331=EDGE_CURVE('',#5801,#5800,#917,.T.);
#7332=EDGE_CURVE('',#5799,#5803,#4843,.T.);
#7333=EDGE_CURVE('',#5799,#5804,#3358,.T.);
#7334=EDGE_CURVE('',#5804,#5804,#4844,.T.);
#7335=EDGE_CURVE('',#5803,#5799,#4845,.T.);
#7336=EDGE_CURVE('',#5805,#5805,#4846,.T.);
#7337=EDGE_CURVE('',#5805,#5798,#3359,.T.);
#7338=EDGE_CURVE('',#5798,#5799,#918,.T.);
#7339=EDGE_CURVE('',#5802,#5803,#919,.T.);
#7340=EDGE_CURVE('',#5806,#5806,#4847,.T.);
#7341=EDGE_CURVE('',#5806,#5805,#4848,.T.);
#7342=EDGE_CURVE('',#5807,#5808,#4849,.T.);
#7343=EDGE_CURVE('',#5808,#5807,#4850,.T.);
#7344=EDGE_CURVE('',#5808,#5809,#3360,.T.);
#7345=EDGE_CURVE('',#5809,#5809,#4851,.T.);
#7346=EDGE_CURVE('',#5807,#5810,#3361,.T.);
#7347=EDGE_CURVE('',#5810,#5810,#4852,.T.);
#7348=EDGE_CURVE('',#5811,#5811,#4853,.T.);
#7349=EDGE_CURVE('',#5811,#5812,#4854,.T.);
#7350=EDGE_CURVE('',#5812,#5812,#4855,.T.);
#7351=EDGE_CURVE('',#5813,#5813,#4856,.T.);
#7352=EDGE_CURVE('',#5813,#5814,#4857,.T.);
#7353=EDGE_CURVE('',#5814,#5814,#4858,.T.);
#7354=EDGE_CURVE('',#5815,#5816,#4859,.T.);
#7355=EDGE_CURVE('',#5816,#5815,#4860,.T.);
#7356=EDGE_CURVE('',#5816,#5817,#4861,.T.);
#7357=EDGE_CURVE('',#5818,#5819,#4862,.T.);
#7358=EDGE_CURVE('',#5819,#5818,#4863,.T.);
#7359=EDGE_CURVE('',#5820,#5819,#4864,.T.);
#7360=EDGE_CURVE('',#5815,#5821,#3362,.T.);
#7361=EDGE_CURVE('',#5822,#5821,#4865,.T.);
#7362=EDGE_CURVE('',#5821,#5822,#4866,.T.);
#7363=EDGE_CURVE('',#5822,#5823,#4867,.T.);
#7364=EDGE_CURVE('',#5823,#5811,#3363,.T.);
#7365=EDGE_CURVE('',#5823,#5822,#4868,.T.);
#7366=EDGE_CURVE('',#5812,#5824,#3364,.T.);
#7367=EDGE_CURVE('',#5825,#5824,#4869,.T.);
#7368=EDGE_CURVE('',#5824,#5825,#4870,.T.);
#7369=EDGE_CURVE('',#5825,#5826,#4871,.T.);
#7370=EDGE_CURVE('',#5826,#5813,#3365,.T.);
#7371=EDGE_CURVE('',#5826,#5825,#4872,.T.);
#7372=EDGE_CURVE('',#5814,#5818,#3366,.T.);
#7373=EDGE_CURVE('',#5827,#5827,#4873,.T.);
#7374=EDGE_CURVE('',#5827,#5828,#4874,.T.);
#7375=EDGE_CURVE('',#5828,#5828,#4875,.T.);
#7376=EDGE_CURVE('',#5829,#5829,#4876,.T.);
#7377=EDGE_CURVE('',#5829,#5830,#4877,.T.);
#7378=EDGE_CURVE('',#5830,#5830,#4878,.T.);
#7379=EDGE_CURVE('',#5831,#5832,#4879,.T.);
#7380=EDGE_CURVE('',#5832,#5831,#4880,.T.);
#7381=EDGE_CURVE('',#5833,#5832,#4881,.T.);
#7382=EDGE_CURVE('',#5834,#5835,#4882,.T.);
#7383=EDGE_CURVE('',#5836,#5834,#4883,.T.);
#7384=EDGE_CURVE('',#5835,#5834,#4884,.T.);
#7385=EDGE_CURVE('',#5831,#5837,#3367,.T.);
#7386=EDGE_CURVE('',#5838,#5837,#4885,.T.);
#7387=EDGE_CURVE('',#5837,#5838,#4886,.T.);
#7388=EDGE_CURVE('',#5838,#5839,#4887,.T.);
#7389=EDGE_CURVE('',#5839,#5827,#3368,.T.);
#7390=EDGE_CURVE('',#5839,#5838,#4888,.T.);
#7391=EDGE_CURVE('',#5828,#5840,#3369,.T.);
#7392=EDGE_CURVE('',#5841,#5840,#4889,.T.);
#7393=EDGE_CURVE('',#5840,#5841,#4890,.T.);
#7394=EDGE_CURVE('',#5841,#5842,#4891,.T.);
#7395=EDGE_CURVE('',#5842,#5829,#3370,.T.);
#7396=EDGE_CURVE('',#5842,#5841,#4892,.T.);
#7397=EDGE_CURVE('',#5830,#5835,#3371,.T.);
#7398=EDGE_CURVE('',#5843,#5843,#4893,.T.);
#7399=EDGE_CURVE('',#5843,#5844,#3372,.T.);
#7400=EDGE_CURVE('',#5844,#5844,#4894,.T.);
#7401=EDGE_CURVE('',#5845,#5845,#4895,.T.);
#7402=EDGE_CURVE('',#5845,#5846,#3373,.T.);
#7403=EDGE_CURVE('',#5846,#5846,#4896,.T.);
#7404=EDGE_CURVE('',#5847,#5847,#4897,.T.);
#7405=EDGE_CURVE('',#5847,#5848,#3374,.T.);
#7406=EDGE_CURVE('',#5848,#5848,#4898,.T.);
#7407=EDGE_CURVE('',#5849,#5849,#4899,.T.);
#7408=EDGE_CURVE('',#5849,#5850,#3375,.T.);
#7409=EDGE_CURVE('',#5850,#5850,#4900,.T.);
#7410=EDGE_CURVE('',#5851,#5851,#4901,.T.);
#7411=EDGE_CURVE('',#5851,#5852,#3376,.T.);
#7412=EDGE_CURVE('',#5852,#5853,#4902,.T.);
#7413=EDGE_CURVE('',#5854,#5853,#3377,.T.);
#7414=EDGE_CURVE('',#5855,#5854,#4903,.T.);
#7415=EDGE_CURVE('',#5855,#5856,#3378,.T.);
#7416=EDGE_CURVE('',#5857,#5856,#4904,.T.);
#7417=EDGE_CURVE('',#5858,#5857,#3379,.T.);
#7418=EDGE_CURVE('',#5859,#5858,#4905,.T.);
#7419=EDGE_CURVE('',#5860,#5859,#3380,.T.);
#7420=EDGE_CURVE('',#5860,#5852,#4906,.T.);
#7421=EDGE_CURVE('',#5861,#5862,#4907,.T.);
#7422=EDGE_CURVE('',#5862,#5863,#920,.T.);
#7423=EDGE_CURVE('',#5864,#5863,#3381,.T.);
#7424=EDGE_CURVE('',#5865,#5864,#4908,.T.);
#7425=EDGE_CURVE('',#5865,#5866,#3382,.T.);
#7426=EDGE_CURVE('',#5866,#5867,#4909,.T.);
#7427=EDGE_CURVE('',#5868,#5867,#4910,.T.);
#7428=EDGE_CURVE('',#5868,#5869,#3383,.T.);
#7429=EDGE_CURVE('',#5869,#5869,#4911,.T.);
#7430=EDGE_CURVE('',#5870,#5868,#4912,.T.);
#7431=EDGE_CURVE('',#5871,#5870,#4913,.T.);
#7432=EDGE_CURVE('',#5871,#5872,#3384,.T.);
#7433=EDGE_CURVE('',#5873,#5872,#4914,.T.);
#7434=EDGE_CURVE('',#5873,#5874,#3385,.T.);
#7435=EDGE_CURVE('',#5874,#5861,#921,.T.);
#7436=EDGE_CURVE('',#5859,#5875,#3386,.T.);
#7437=EDGE_CURVE('',#5872,#5859,#3387,.T.);
#7438=EDGE_CURVE('',#5872,#5876,#3388,.T.);
#7439=EDGE_CURVE('',#5876,#5875,#3389,.T.);
#7440=EDGE_CURVE('',#5854,#5865,#3390,.T.);
#7441=EDGE_CURVE('',#5854,#5877,#3391,.T.);
#7442=EDGE_CURVE('',#5878,#5877,#3392,.T.);
#7443=EDGE_CURVE('',#5865,#5878,#3393,.T.);
#7444=EDGE_CURVE('',#5853,#5867,#3394,.T.);
#7445=EDGE_CURVE('',#5860,#5870,#3395,.T.);
#7446=EDGE_CURVE('',#5871,#5879,#3396,.T.);
#7447=EDGE_CURVE('',#5870,#5880,#3397,.T.);
#7448=EDGE_CURVE('',#5879,#5880,#3398,.T.);
#7449=EDGE_CURVE('',#5880,#5881,#3399,.T.);
#7450=EDGE_CURVE('',#5882,#5881,#3400,.T.);
#7451=EDGE_CURVE('',#5879,#5882,#3401,.T.);
#7452=EDGE_CURVE('',#5881,#5883,#3402,.T.);
#7453=EDGE_CURVE('',#5884,#5883,#3403,.T.);
#7454=EDGE_CURVE('',#5882,#5884,#3404,.T.);
#7455=EDGE_CURVE('',#5875,#5883,#3405,.T.);
#7456=EDGE_CURVE('',#5876,#5884,#3406,.T.);
#7457=EDGE_CURVE('',#5866,#5885,#3407,.T.);
#7458=EDGE_CURVE('',#5885,#5886,#3408,.T.);
#7459=EDGE_CURVE('',#5867,#5886,#3409,.T.);
#7460=EDGE_CURVE('',#5886,#5887,#3410,.T.);
#7461=EDGE_CURVE('',#5885,#5888,#3411,.T.);
#7462=EDGE_CURVE('',#5888,#5887,#3412,.T.);
#7463=EDGE_CURVE('',#5877,#5889,#3413,.T.);
#7464=EDGE_CURVE('',#5890,#5889,#3414,.T.);
#7465=EDGE_CURVE('',#5878,#5890,#3415,.T.);
#7466=EDGE_CURVE('',#5887,#5889,#3416,.T.);
#7467=EDGE_CURVE('',#5888,#5890,#3417,.T.);
#7468=EDGE_CURVE('',#5857,#5856,#4915,.T.);
#7469=EDGE_CURVE('',#5858,#5855,#4916,.T.);
#7470=EDGE_CURVE('',#5863,#5874,#922,.T.);
#7471=EDGE_CURVE('',#5864,#5873,#4917,.T.);
#7472=EDGE_CURVE('',#5861,#5862,#923,.T.);
#7473=EDGE_CURVE('',#5891,#5892,#4918,.T.);
#7474=EDGE_CURVE('',#5892,#5891,#4919,.T.);
#7475=EDGE_CURVE('',#5892,#5893,#4920,.T.);
#7476=EDGE_CURVE('',#5894,#5893,#4921,.T.);
#7477=EDGE_CURVE('',#5893,#5894,#4922,.T.);
#7478=EDGE_CURVE('',#5891,#5895,#3418,.T.);
#7479=EDGE_CURVE('',#5895,#5895,#4923,.T.);
#7480=EDGE_CURVE('',#5896,#5896,#4924,.T.);
#7481=EDGE_CURVE('',#5896,#5894,#3419,.T.);
#7482=EDGE_CURVE('',#5897,#5897,#4925,.T.);
#7483=EDGE_CURVE('',#5897,#5898,#4926,.T.);
#7484=EDGE_CURVE('',#5899,#5898,#4927,.T.);
#7485=EDGE_CURVE('',#5898,#5899,#4928,.T.);
#7486=EDGE_CURVE('',#5900,#5901,#4929,.T.);
#7487=EDGE_CURVE('',#5901,#5900,#4930,.T.);
#7488=EDGE_CURVE('',#5901,#5902,#4931,.T.);
#7489=EDGE_CURVE('',#5902,#5902,#4932,.T.);
#7490=EDGE_CURVE('',#5900,#5899,#3420,.T.);
#7491=EDGE_CURVE('',#5903,#5903,#4933,.T.);
#7492=EDGE_CURVE('',#5903,#5904,#3421,.T.);
#7493=EDGE_CURVE('',#5904,#5904,#4934,.T.);
#7494=EDGE_CURVE('',#5905,#5905,#4935,.T.);
#7495=EDGE_CURVE('',#5905,#5906,#3422,.T.);
#7496=EDGE_CURVE('',#5906,#5906,#4936,.T.);
#7497=EDGE_CURVE('',#5907,#5908,#4937,.T.);
#7498=EDGE_CURVE('',#5908,#5907,#4938,.T.);
#7499=EDGE_CURVE('',#5908,#5909,#3423,.T.);
#7500=EDGE_CURVE('',#5909,#5909,#4939,.T.);
#7501=EDGE_CURVE('',#5907,#5905,#3424,.T.);
#7502=EDGE_CURVE('',#5910,#5911,#4940,.T.);
#7503=EDGE_CURVE('',#5911,#5910,#4941,.T.);
#7504=EDGE_CURVE('',#5911,#5912,#3425,.T.);
#7505=EDGE_CURVE('',#5912,#5912,#4942,.T.);
#7506=EDGE_CURVE('',#5913,#5913,#4943,.T.);
#7507=EDGE_CURVE('',#5913,#5914,#3426,.T.);
#7508=EDGE_CURVE('',#5914,#5914,#4944,.T.);
#7509=EDGE_CURVE('',#5915,#5915,#4945,.T.);
#7510=EDGE_CURVE('',#5915,#5916,#4946,.T.);
#7511=EDGE_CURVE('',#5917,#5916,#4947,.T.);
#7512=EDGE_CURVE('',#5916,#5917,#4948,.T.);
#7513=EDGE_CURVE('',#5918,#5918,#4949,.T.);
#7514=EDGE_CURVE('',#5918,#5919,#4950,.T.);
#7515=EDGE_CURVE('',#5919,#5919,#4951,.T.);
#7516=EDGE_CURVE('',#5920,#5921,#4952,.T.);
#7517=EDGE_CURVE('',#5921,#5920,#4953,.T.);
#7518=EDGE_CURVE('',#5921,#5922,#4954,.T.);
#7519=EDGE_CURVE('',#5922,#5922,#4955,.T.);
#7520=EDGE_CURVE('',#5923,#5923,#4956,.T.);
#7521=EDGE_CURVE('',#5923,#5924,#4957,.T.);
#7522=EDGE_CURVE('',#5925,#5924,#4958,.T.);
#7523=EDGE_CURVE('',#5924,#5925,#4959,.T.);
#7524=EDGE_CURVE('',#5926,#5926,#4960,.T.);
#7525=EDGE_CURVE('',#5926,#5927,#3427,.T.);
#7526=EDGE_CURVE('',#5927,#5927,#4961,.T.);
#7527=EDGE_CURVE('',#5928,#5928,#4962,.T.);
#7528=EDGE_CURVE('',#5928,#5929,#3428,.T.);
#7529=EDGE_CURVE('',#5929,#5929,#4963,.T.);
#7530=EDGE_CURVE('',#5919,#5913,#3429,.T.);
#7531=EDGE_CURVE('',#5930,#5930,#4964,.T.);
#7532=EDGE_CURVE('',#5930,#5931,#3430,.T.);
#7533=EDGE_CURVE('',#5931,#5931,#4965,.T.);
#7534=EDGE_CURVE('',#5910,#5925,#3431,.T.);
#7535=EDGE_CURVE('',#5920,#5917,#3432,.T.);
#7536=EDGE_CURVE('',#5932,#5933,#4966,.T.);
#7537=EDGE_CURVE('',#5933,#5932,#4967,.T.);
#7538=EDGE_CURVE('',#5933,#5934,#3433,.T.);
#7539=EDGE_CURVE('',#5934,#5934,#4968,.T.);
#7540=EDGE_CURVE('',#5935,#5935,#4969,.T.);
#7541=EDGE_CURVE('',#5935,#5936,#3434,.T.);
#7542=EDGE_CURVE('',#5936,#5936,#4970,.T.);
#7543=EDGE_CURVE('',#5937,#5937,#4971,.T.);
#7544=EDGE_CURVE('',#5937,#5938,#4972,.T.);
#7545=EDGE_CURVE('',#5939,#5938,#4973,.T.);
#7546=EDGE_CURVE('',#5938,#5939,#4974,.T.);
#7547=EDGE_CURVE('',#5940,#5940,#4975,.T.);
#7548=EDGE_CURVE('',#5940,#5941,#4976,.T.);
#7549=EDGE_CURVE('',#5941,#5941,#4977,.T.);
#7550=EDGE_CURVE('',#5942,#5943,#4978,.T.);
#7551=EDGE_CURVE('',#5943,#5942,#4979,.T.);
#7552=EDGE_CURVE('',#5943,#5944,#4980,.T.);
#7553=EDGE_CURVE('',#5944,#5944,#4981,.T.);
#7554=EDGE_CURVE('',#5945,#5945,#4982,.T.);
#7555=EDGE_CURVE('',#5945,#5946,#4983,.T.);
#7556=EDGE_CURVE('',#5947,#5946,#4984,.T.);
#7557=EDGE_CURVE('',#5946,#5947,#4985,.T.);
#7558=EDGE_CURVE('',#5948,#5948,#4986,.T.);
#7559=EDGE_CURVE('',#5948,#5949,#3435,.T.);
#7560=EDGE_CURVE('',#5949,#5949,#4987,.T.);
#7561=EDGE_CURVE('',#5950,#5950,#4988,.T.);
#7562=EDGE_CURVE('',#5950,#5951,#3436,.T.);
#7563=EDGE_CURVE('',#5951,#5951,#4989,.T.);
#7564=EDGE_CURVE('',#5941,#5935,#3437,.T.);
#7565=EDGE_CURVE('',#5952,#5952,#4990,.T.);
#7566=EDGE_CURVE('',#5952,#5953,#3438,.T.);
#7567=EDGE_CURVE('',#5953,#5953,#4991,.T.);
#7568=EDGE_CURVE('',#5932,#5947,#3439,.T.);
#7569=EDGE_CURVE('',#5942,#5939,#3440,.T.);
#7570=EDGE_CURVE('',#5954,#5954,#4992,.T.);
#7571=EDGE_CURVE('',#5954,#5955,#3441,.T.);
#7572=EDGE_CURVE('',#5955,#5955,#4993,.T.);
#7573=EDGE_CURVE('',#5956,#5957,#4994,.T.);
#7574=EDGE_CURVE('',#5957,#5956,#4995,.T.);
#7575=EDGE_CURVE('',#5957,#5958,#3442,.T.);
#7576=EDGE_CURVE('',#5958,#5958,#4996,.T.);
#7577=EDGE_CURVE('',#5956,#5954,#3443,.T.);
#7578=EDGE_CURVE('',#5959,#5960,#3444,.T.);
#7579=EDGE_CURVE('',#5959,#5961,#36,.T.);
#7580=EDGE_CURVE('',#5961,#5962,#3445,.T.);
#7581=EDGE_CURVE('',#5960,#5962,#37,.T.);
#7582=EDGE_CURVE('',#5963,#5964,#3446,.T.);
#7583=EDGE_CURVE('',#5963,#5959,#38,.T.);
#7584=EDGE_CURVE('',#5964,#5960,#39,.T.);
#7585=EDGE_CURVE('',#5965,#5966,#3447,.T.);
#7586=EDGE_CURVE('',#5965,#5963,#40,.T.);
#7587=EDGE_CURVE('',#5966,#5964,#41,.T.);
#7588=EDGE_CURVE('',#5967,#5968,#3448,.T.);
#7589=EDGE_CURVE('',#5967,#5965,#42,.T.);
#7590=EDGE_CURVE('',#5968,#5966,#43,.T.);
#7591=EDGE_CURVE('',#5969,#5970,#3449,.T.);
#7592=EDGE_CURVE('',#5969,#5967,#44,.T.);
#7593=EDGE_CURVE('',#5970,#5968,#45,.T.);
#7594=EDGE_CURVE('',#5971,#5972,#3450,.T.);
#7595=EDGE_CURVE('',#5971,#5969,#46,.T.);
#7596=EDGE_CURVE('',#5972,#5970,#47,.T.);
#7597=EDGE_CURVE('',#5973,#5974,#3451,.T.);
#7598=EDGE_CURVE('',#5973,#5971,#48,.T.);
#7599=EDGE_CURVE('',#5974,#5972,#49,.T.);
#7600=EDGE_CURVE('',#5975,#5976,#3452,.T.);
#7601=EDGE_CURVE('',#5975,#5973,#50,.T.);
#7602=EDGE_CURVE('',#5976,#5974,#51,.T.);
#7603=EDGE_CURVE('',#5977,#5978,#3453,.T.);
#7604=EDGE_CURVE('',#5977,#5975,#52,.T.);
#7605=EDGE_CURVE('',#5978,#5976,#53,.T.);
#7606=EDGE_CURVE('',#5979,#5980,#3454,.T.);
#7607=EDGE_CURVE('',#5979,#5977,#54,.T.);
#7608=EDGE_CURVE('',#5980,#5978,#55,.T.);
#7609=EDGE_CURVE('',#5981,#5982,#3455,.T.);
#7610=EDGE_CURVE('',#5981,#5979,#56,.T.);
#7611=EDGE_CURVE('',#5982,#5980,#57,.T.);
#7612=EDGE_CURVE('',#5983,#5984,#3456,.T.);
#7613=EDGE_CURVE('',#5983,#5981,#58,.T.);
#7614=EDGE_CURVE('',#5984,#5982,#59,.T.);
#7615=EDGE_CURVE('',#5985,#5986,#3457,.T.);
#7616=EDGE_CURVE('',#5985,#5983,#60,.T.);
#7617=EDGE_CURVE('',#5986,#5984,#61,.T.);
#7618=EDGE_CURVE('',#5987,#5988,#3458,.T.);
#7619=EDGE_CURVE('',#5987,#5989,#924,.T.);
#7620=EDGE_CURVE('',#5989,#5990,#3459,.T.);
#7621=EDGE_CURVE('',#5990,#5990,#4997,.T.);
#7622=EDGE_CURVE('',#5989,#5991,#925,.T.);
#7623=EDGE_CURVE('',#5991,#5992,#3460,.T.);
#7624=EDGE_CURVE('',#5988,#5992,#926,.F.);
#7625=EDGE_CURVE('',#5993,#5994,#3461,.T.);
#7626=EDGE_CURVE('',#5993,#5987,#927,.T.);
#7627=EDGE_CURVE('',#5994,#5988,#928,.F.);
#7628=EDGE_CURVE('',#5995,#5996,#3462,.T.);
#7629=EDGE_CURVE('',#5995,#5993,#929,.T.);
#7630=EDGE_CURVE('',#5996,#5994,#930,.F.);
#7631=EDGE_CURVE('',#5997,#5998,#3463,.T.);
#7632=EDGE_CURVE('',#5997,#5995,#931,.T.);
#7633=EDGE_CURVE('',#5998,#5996,#932,.F.);
#7634=EDGE_CURVE('',#5999,#6000,#3464,.T.);
#7635=EDGE_CURVE('',#5999,#5997,#933,.T.);
#7636=EDGE_CURVE('',#6000,#5998,#934,.F.);
#7637=EDGE_CURVE('',#6001,#6002,#3465,.T.);
#7638=EDGE_CURVE('',#6001,#5999,#935,.T.);
#7639=EDGE_CURVE('',#6002,#6000,#936,.F.);
#7640=EDGE_CURVE('',#6003,#6004,#3466,.T.);
#7641=EDGE_CURVE('',#6003,#6001,#937,.T.);
#7642=EDGE_CURVE('',#6004,#6002,#938,.F.);
#7643=EDGE_CURVE('',#6005,#6006,#3467,.T.);
#7644=EDGE_CURVE('',#6005,#6003,#939,.T.);
#7645=EDGE_CURVE('',#6006,#6004,#940,.F.);
#7646=EDGE_CURVE('',#6007,#6008,#3468,.T.);
#7647=EDGE_CURVE('',#6007,#6005,#941,.T.);
#7648=EDGE_CURVE('',#6008,#6006,#942,.F.);
#7649=EDGE_CURVE('',#6009,#6010,#3469,.T.);
#7650=EDGE_CURVE('',#6009,#6007,#943,.T.);
#7651=EDGE_CURVE('',#6010,#6008,#944,.F.);
#7652=EDGE_CURVE('',#6011,#6012,#3470,.T.);
#7653=EDGE_CURVE('',#6011,#6009,#945,.T.);
#7654=EDGE_CURVE('',#6012,#6010,#946,.F.);
#7655=EDGE_CURVE('',#6013,#6014,#3471,.T.);
#7656=EDGE_CURVE('',#6013,#6011,#947,.T.);
#7657=EDGE_CURVE('',#6014,#6012,#948,.F.);
#7658=EDGE_CURVE('',#6015,#6014,#949,.F.);
#7659=EDGE_CURVE('',#6015,#6016,#4998,.T.);
#7660=EDGE_CURVE('',#6016,#6013,#950,.T.);
#7661=EDGE_CURVE('',#6017,#6017,#4999,.T.);
#7662=EDGE_CURVE('',#6017,#6018,#3472,.T.);
#7663=EDGE_CURVE('',#6018,#6019,#5000,.T.);
#7664=EDGE_CURVE('',#6019,#6020,#5001,.T.);
#7665=EDGE_CURVE('',#6020,#6021,#5002,.T.);
#7666=EDGE_CURVE('',#6021,#6018,#5003,.T.);
#7667=EDGE_CURVE('',#6022,#6022,#5004,.T.);
#7668=EDGE_CURVE('',#6022,#6023,#3473,.T.);
#7669=EDGE_CURVE('',#6023,#6023,#5005,.T.);
#7670=EDGE_CURVE('',#6024,#6024,#5006,.T.);
#7671=EDGE_CURVE('',#6024,#6025,#3474,.T.);
#7672=EDGE_CURVE('',#6025,#6025,#5007,.T.);
#7673=EDGE_CURVE('',#6015,#6026,#951,.T.);
#7674=EDGE_CURVE('',#6026,#6027,#3475,.T.);
#7675=EDGE_CURVE('',#6027,#6027,#5008,.T.);
#7676=EDGE_CURVE('',#6026,#6028,#952,.T.);
#7677=EDGE_CURVE('',#6028,#6029,#5009,.T.);
#7678=EDGE_CURVE('',#6029,#6016,#953,.T.);
#7679=EDGE_CURVE('',#6030,#6031,#3476,.T.);
#7680=EDGE_CURVE('',#6031,#6019,#3477,.T.);
#7681=EDGE_CURVE('',#6021,#6030,#3478,.T.);
#7682=EDGE_CURVE('',#6032,#6020,#3479,.T.);
#7683=EDGE_CURVE('',#6032,#6021,#3480,.T.);
#7684=EDGE_CURVE('',#6033,#6034,#3481,.T.);
#7685=EDGE_CURVE('',#6033,#6035,#3482,.T.);
#7686=EDGE_CURVE('',#6036,#6035,#3483,.T.);
#7687=EDGE_CURVE('',#6034,#6036,#5010,.T.);
#7688=EDGE_CURVE('',#6037,#6038,#3484,.T.);
#7689=EDGE_CURVE('',#6038,#6039,#3485,.T.);
#7690=EDGE_CURVE('',#6039,#6040,#3486,.T.);
#7691=EDGE_CURVE('',#6040,#6037,#5011,.T.);
#7692=EDGE_CURVE('',#6019,#6041,#3487,.T.);
#7693=EDGE_CURVE('',#6020,#6041,#3488,.T.);
#7694=EDGE_CURVE('',#6042,#6043,#3489,.T.);
#7695=EDGE_CURVE('',#6042,#6044,#3490,.T.);
#7696=EDGE_CURVE('',#6045,#6044,#3491,.T.);
#7697=EDGE_CURVE('',#6043,#6045,#5012,.T.);
#7698=EDGE_CURVE('',#6046,#6047,#3492,.T.);
#7699=EDGE_CURVE('',#6046,#6048,#3493,.T.);
#7700=EDGE_CURVE('',#6049,#6048,#3494,.T.);
#7701=EDGE_CURVE('',#6047,#6049,#5013,.T.);
#7702=EDGE_CURVE('',#6050,#6051,#3495,.T.);
#7703=EDGE_CURVE('',#6051,#6052,#3496,.T.);
#7704=EDGE_CURVE('',#6053,#6052,#3497,.T.);
#7705=EDGE_CURVE('',#6053,#6050,#3498,.T.);
#7706=EDGE_CURVE('',#6054,#6050,#3499,.T.);
#7707=EDGE_CURVE('',#6054,#6031,#5014,.T.);
#7708=EDGE_CURVE('',#6030,#6055,#5015,.T.);
#7709=EDGE_CURVE('',#6051,#6055,#3500,.T.);
#7710=EDGE_CURVE('',#6041,#6056,#5016,.T.);
#7711=EDGE_CURVE('',#6056,#6053,#3501,.T.);
#7712=EDGE_CURVE('',#6052,#6057,#3502,.T.);
#7713=EDGE_CURVE('',#6057,#6032,#5017,.T.);
#7714=EDGE_CURVE('',#6044,#6057,#803,.T.);
#7715=EDGE_CURVE('',#6052,#6046,#804,.T.);
#7716=EDGE_CURVE('',#6047,#6045,#3503,.T.);
#7717=EDGE_CURVE('',#6055,#6042,#805,.T.);
#7718=EDGE_CURVE('',#6049,#6043,#3504,.T.);
#7719=EDGE_CURVE('',#6048,#6051,#806,.T.);
#7720=EDGE_CURVE('',#6037,#6036,#3505,.T.);
#7721=EDGE_CURVE('',#6040,#6034,#3506,.T.);
#7722=EDGE_CURVE('',#6039,#6054,#807,.T.);
#7723=EDGE_CURVE('',#6050,#6033,#808,.T.);
#7724=EDGE_CURVE('',#6056,#6038,#809,.T.);
#7725=EDGE_CURVE('',#6035,#6053,#810,.T.);
#7726=EDGE_CURVE('',#5992,#5961,#3507,.T.);
#7727=EDGE_CURVE('',#5962,#5991,#3508,.T.);
#7728=EDGE_CURVE('',#6028,#5985,#62,.T.);
#7729=EDGE_CURVE('',#6029,#5986,#63,.T.);
#7730=EDGE_CURVE('',#6058,#6059,#3509,.T.);
#7731=EDGE_CURVE('',#6060,#6059,#64,.T.);
#7732=EDGE_CURVE('',#6061,#6060,#5018,.T.);
#7733=EDGE_CURVE('',#6061,#6058,#65,.T.);
#7734=EDGE_CURVE('',#6062,#6063,#3510,.T.);
#7735=EDGE_CURVE('',#6059,#6063,#66,.T.);
#7736=EDGE_CURVE('',#6058,#6062,#67,.T.);
#7737=EDGE_CURVE('',#6064,#6065,#3511,.T.);
#7738=EDGE_CURVE('',#6063,#6065,#68,.T.);
#7739=EDGE_CURVE('',#6062,#6064,#69,.T.);
#7740=EDGE_CURVE('',#6066,#6067,#3512,.T.);
#7741=EDGE_CURVE('',#6065,#6067,#70,.T.);
#7742=EDGE_CURVE('',#6064,#6066,#71,.T.);
#7743=EDGE_CURVE('',#6068,#6069,#3513,.T.);
#7744=EDGE_CURVE('',#6067,#6069,#72,.T.);
#7745=EDGE_CURVE('',#6066,#6068,#73,.T.);
#7746=EDGE_CURVE('',#6070,#6071,#3514,.T.);
#7747=EDGE_CURVE('',#6069,#6071,#74,.T.);
#7748=EDGE_CURVE('',#6068,#6070,#75,.T.);
#7749=EDGE_CURVE('',#6072,#6073,#3515,.T.);
#7750=EDGE_CURVE('',#6071,#6073,#76,.T.);
#7751=EDGE_CURVE('',#6070,#6072,#77,.T.);
#7752=EDGE_CURVE('',#6074,#6075,#3516,.T.);
#7753=EDGE_CURVE('',#6074,#6076,#78,.T.);
#7754=EDGE_CURVE('',#6076,#6077,#3517,.T.);
#7755=EDGE_CURVE('',#6075,#6077,#79,.T.);
#7756=EDGE_CURVE('',#6078,#6079,#3518,.T.);
#7757=EDGE_CURVE('',#6079,#6080,#954,.T.);
#7758=EDGE_CURVE('',#6080,#6081,#3519,.T.);
#7759=EDGE_CURVE('',#6082,#6081,#955,.F.);
#7760=EDGE_CURVE('',#6082,#6083,#3520,.T.);
#7761=EDGE_CURVE('',#6083,#6083,#5019,.T.);
#7762=EDGE_CURVE('',#6078,#6082,#956,.F.);
#7763=EDGE_CURVE('',#6084,#6085,#3521,.T.);
#7764=EDGE_CURVE('',#6085,#6079,#957,.T.);
#7765=EDGE_CURVE('',#6084,#6078,#958,.F.);
#7766=EDGE_CURVE('',#6086,#6087,#3522,.T.);
#7767=EDGE_CURVE('',#6087,#6085,#959,.T.);
#7768=EDGE_CURVE('',#6086,#6084,#960,.F.);
#7769=EDGE_CURVE('',#6088,#6089,#3523,.T.);
#7770=EDGE_CURVE('',#6089,#6087,#961,.T.);
#7771=EDGE_CURVE('',#6088,#6086,#962,.F.);
#7772=EDGE_CURVE('',#6090,#6091,#3524,.T.);
#7773=EDGE_CURVE('',#6091,#6089,#963,.T.);
#7774=EDGE_CURVE('',#6090,#6088,#964,.F.);
#7775=EDGE_CURVE('',#6092,#6093,#3525,.T.);
#7776=EDGE_CURVE('',#6093,#6091,#965,.T.);
#7777=EDGE_CURVE('',#6092,#6090,#966,.F.);
#7778=EDGE_CURVE('',#6094,#6095,#3526,.T.);
#7779=EDGE_CURVE('',#6095,#6093,#967,.T.);
#7780=EDGE_CURVE('',#6094,#6092,#968,.F.);
#7781=EDGE_CURVE('',#6096,#6097,#3527,.T.);
#7782=EDGE_CURVE('',#6098,#6096,#969,.F.);
#7783=EDGE_CURVE('',#6098,#6099,#5020,.T.);
#7784=EDGE_CURVE('',#6099,#6097,#970,.T.);
#7785=EDGE_CURVE('',#6097,#6095,#971,.T.);
#7786=EDGE_CURVE('',#6096,#6094,#972,.F.);
#7787=EDGE_CURVE('',#6100,#6100,#5021,.T.);
#7788=EDGE_CURVE('',#6100,#6101,#3528,.T.);
#7789=EDGE_CURVE('',#6101,#6101,#5022,.T.);
#7790=EDGE_CURVE('',#6102,#6103,#3529,.T.);
#7791=EDGE_CURVE('',#6103,#6104,#3530,.T.);
#7792=EDGE_CURVE('',#6104,#6105,#3531,.T.);
#7793=EDGE_CURVE('',#6105,#6106,#3532,.T.);
#7794=EDGE_CURVE('',#6106,#6107,#3533,.T.);
#7795=EDGE_CURVE('',#6107,#6108,#3534,.T.);
#7796=EDGE_CURVE('',#6108,#6109,#3535,.T.);
#7797=EDGE_CURVE('',#6109,#6110,#3536,.T.);
#7798=EDGE_CURVE('',#6110,#6111,#3537,.T.);
#7799=EDGE_CURVE('',#6111,#6112,#3538,.T.);
#7800=EDGE_CURVE('',#6112,#6113,#3539,.T.);
#7801=EDGE_CURVE('',#6113,#6102,#3540,.T.);
#7802=EDGE_CURVE('',#6060,#6099,#973,.T.);
#7803=EDGE_CURVE('',#6098,#6061,#974,.T.);
#7804=EDGE_CURVE('',#6114,#6115,#3541,.T.);
#7805=EDGE_CURVE('',#6116,#6114,#3542,.T.);
#7806=EDGE_CURVE('',#6117,#6116,#3543,.T.);
#7807=EDGE_CURVE('',#6118,#6117,#3544,.T.);
#7808=EDGE_CURVE('',#6119,#6118,#3545,.T.);
#7809=EDGE_CURVE('',#6115,#6119,#3546,.T.);
#7810=EDGE_CURVE('',#6103,#6120,#3547,.T.);
#7811=EDGE_CURVE('',#6121,#6102,#3548,.T.);
#7812=EDGE_CURVE('',#6121,#6114,#3549,.T.);
#7813=EDGE_CURVE('',#6120,#6115,#3550,.T.);
#7814=EDGE_CURVE('',#6120,#6104,#3551,.T.);
#7815=EDGE_CURVE('',#6122,#6119,#3552,.T.);
#7816=EDGE_CURVE('',#6105,#6122,#3553,.T.);
#7817=EDGE_CURVE('',#6107,#6123,#3554,.T.);
#7818=EDGE_CURVE('',#6122,#6106,#3555,.T.);
#7819=EDGE_CURVE('',#6123,#6118,#3556,.T.);
#7820=EDGE_CURVE('',#6123,#6108,#3557,.T.);
#7821=EDGE_CURVE('',#6124,#6117,#3558,.T.);
#7822=EDGE_CURVE('',#6109,#6124,#3559,.T.);
#7823=EDGE_CURVE('',#6111,#6125,#3560,.T.);
#7824=EDGE_CURVE('',#6124,#6110,#3561,.T.);
#7825=EDGE_CURVE('',#6125,#6116,#3562,.T.);
#7826=EDGE_CURVE('',#6113,#6121,#3563,.T.);
#7827=EDGE_CURVE('',#6125,#6112,#3564,.T.);
#7828=EDGE_CURVE('',#6081,#6076,#3565,.T.);
#7829=EDGE_CURVE('',#6077,#6080,#3566,.T.);
#7830=EDGE_CURVE('',#6073,#6075,#80,.T.);
#7831=EDGE_CURVE('',#6072,#6074,#81,.T.);
#7832=EDGE_CURVE('',#6126,#6126,#5023,.T.);
#7833=EDGE_CURVE('',#6126,#6127,#3567,.T.);
#7834=EDGE_CURVE('',#6127,#6127,#5024,.T.);
#7835=EDGE_CURVE('',#6128,#6129,#5025,.T.);
#7836=EDGE_CURVE('',#6129,#6128,#5026,.T.);
#7837=EDGE_CURVE('',#6129,#6130,#3568,.T.);
#7838=EDGE_CURVE('',#6130,#6130,#5027,.T.);
#7839=EDGE_CURVE('',#6131,#6131,#5028,.T.);
#7840=EDGE_CURVE('',#6131,#6126,#3569,.T.);
#7841=EDGE_CURVE('',#6128,#6132,#3570,.T.);
#7842=EDGE_CURVE('',#6132,#6132,#5029,.T.);
#7843=EDGE_CURVE('',#6133,#6133,#5030,.T.);
#7844=EDGE_CURVE('',#6133,#6134,#3571,.T.);
#7845=EDGE_CURVE('',#6134,#6134,#5031,.T.);
#7846=EDGE_CURVE('',#6135,#6136,#5032,.T.);
#7847=EDGE_CURVE('',#6136,#6135,#5033,.T.);
#7848=EDGE_CURVE('',#6136,#6137,#3572,.T.);
#7849=EDGE_CURVE('',#6137,#6137,#5034,.T.);
#7850=EDGE_CURVE('',#6135,#6133,#3573,.T.);
#7851=ORIENTED_EDGE('',*,*,#6138,.F.);
#7852=ORIENTED_EDGE('',*,*,#6139,.T.);
#7853=ORIENTED_EDGE('',*,*,#6140,.F.);
#7854=ORIENTED_EDGE('',*,*,#6139,.F.);
#7855=ORIENTED_EDGE('',*,*,#6141,.F.);
#7856=ORIENTED_EDGE('',*,*,#6142,.T.);
#7857=ORIENTED_EDGE('',*,*,#6143,.F.);
#7858=ORIENTED_EDGE('',*,*,#6142,.F.);
#7859=ORIENTED_EDGE('',*,*,#6144,.F.);
#7860=ORIENTED_EDGE('',*,*,#6145,.T.);
#7861=ORIENTED_EDGE('',*,*,#6146,.F.);
#7862=ORIENTED_EDGE('',*,*,#6145,.F.);
#7863=ORIENTED_EDGE('',*,*,#6147,.F.);
#7864=ORIENTED_EDGE('',*,*,#6148,.T.);
#7865=ORIENTED_EDGE('',*,*,#6149,.F.);
#7866=ORIENTED_EDGE('',*,*,#6148,.F.);
#7867=ORIENTED_EDGE('',*,*,#6150,.F.);
#7868=ORIENTED_EDGE('',*,*,#6151,.T.);
#7869=ORIENTED_EDGE('',*,*,#6152,.F.);
#7870=ORIENTED_EDGE('',*,*,#6151,.F.);
#7871=ORIENTED_EDGE('',*,*,#6153,.F.);
#7872=ORIENTED_EDGE('',*,*,#6154,.T.);
#7873=ORIENTED_EDGE('',*,*,#6155,.F.);
#7874=ORIENTED_EDGE('',*,*,#6154,.F.);
#7875=ORIENTED_EDGE('',*,*,#6156,.F.);
#7876=ORIENTED_EDGE('',*,*,#6157,.F.);
#7877=ORIENTED_EDGE('',*,*,#6158,.F.);
#7878=ORIENTED_EDGE('',*,*,#6159,.F.);
#7879=ORIENTED_EDGE('',*,*,#6160,.T.);
#7880=ORIENTED_EDGE('',*,*,#6161,.F.);
#7881=ORIENTED_EDGE('',*,*,#6162,.F.);
#7882=ORIENTED_EDGE('',*,*,#6163,.F.);
#7883=ORIENTED_EDGE('',*,*,#6164,.T.);
#7884=ORIENTED_EDGE('',*,*,#6165,.F.);
#7885=ORIENTED_EDGE('',*,*,#6166,.T.);
#7886=ORIENTED_EDGE('',*,*,#6167,.F.);
#7887=ORIENTED_EDGE('',*,*,#6166,.F.);
#7888=ORIENTED_EDGE('',*,*,#6168,.F.);
#7889=ORIENTED_EDGE('',*,*,#6169,.T.);
#7890=ORIENTED_EDGE('',*,*,#6170,.F.);
#7891=ORIENTED_EDGE('',*,*,#6169,.F.);
#7892=ORIENTED_EDGE('',*,*,#6171,.F.);
#7893=ORIENTED_EDGE('',*,*,#6172,.T.);
#7894=ORIENTED_EDGE('',*,*,#6173,.F.);
#7895=ORIENTED_EDGE('',*,*,#6172,.F.);
#7896=ORIENTED_EDGE('',*,*,#6174,.F.);
#7897=ORIENTED_EDGE('',*,*,#6175,.T.);
#7898=ORIENTED_EDGE('',*,*,#6176,.F.);
#7899=ORIENTED_EDGE('',*,*,#6175,.F.);
#7900=ORIENTED_EDGE('',*,*,#6177,.F.);
#7901=ORIENTED_EDGE('',*,*,#6178,.F.);
#7902=ORIENTED_EDGE('',*,*,#6179,.F.);
#7903=ORIENTED_EDGE('',*,*,#6180,.F.);
#7904=ORIENTED_EDGE('',*,*,#6181,.F.);
#7905=ORIENTED_EDGE('',*,*,#6182,.F.);
#7906=ORIENTED_EDGE('',*,*,#6183,.F.);
#7907=ORIENTED_EDGE('',*,*,#6184,.F.);
#7908=ORIENTED_EDGE('',*,*,#6185,.F.);
#7909=ORIENTED_EDGE('',*,*,#6186,.F.);
#7910=ORIENTED_EDGE('',*,*,#6187,.F.);
#7911=ORIENTED_EDGE('',*,*,#6188,.T.);
#7912=ORIENTED_EDGE('',*,*,#6189,.F.);
#7913=ORIENTED_EDGE('',*,*,#6190,.F.);
#7914=ORIENTED_EDGE('',*,*,#6188,.F.);
#7915=ORIENTED_EDGE('',*,*,#6191,.F.);
#7916=ORIENTED_EDGE('',*,*,#6192,.T.);
#7917=ORIENTED_EDGE('',*,*,#6193,.F.);
#7918=ORIENTED_EDGE('',*,*,#6192,.F.);
#7919=ORIENTED_EDGE('',*,*,#6194,.F.);
#7920=ORIENTED_EDGE('',*,*,#6195,.F.);
#7921=ORIENTED_EDGE('',*,*,#6196,.T.);
#7922=ORIENTED_EDGE('',*,*,#6197,.F.);
#7923=ORIENTED_EDGE('',*,*,#6196,.F.);
#7924=ORIENTED_EDGE('',*,*,#6198,.F.);
#7925=ORIENTED_EDGE('',*,*,#6199,.F.);
#7926=ORIENTED_EDGE('',*,*,#6200,.T.);
#7927=ORIENTED_EDGE('',*,*,#6201,.F.);
#7928=ORIENTED_EDGE('',*,*,#6200,.F.);
#7929=ORIENTED_EDGE('',*,*,#6202,.F.);
#7930=ORIENTED_EDGE('',*,*,#6203,.F.);
#7931=ORIENTED_EDGE('',*,*,#6204,.F.);
#7932=ORIENTED_EDGE('',*,*,#6205,.T.);
#7933=ORIENTED_EDGE('',*,*,#6206,.F.);
#7934=ORIENTED_EDGE('',*,*,#6207,.F.);
#7935=ORIENTED_EDGE('',*,*,#6208,.F.);
#7936=ORIENTED_EDGE('',*,*,#6209,.T.);
#7937=ORIENTED_EDGE('',*,*,#6210,.F.);
#7938=ORIENTED_EDGE('',*,*,#6211,.F.);
#7939=ORIENTED_EDGE('',*,*,#6212,.T.);
#7940=ORIENTED_EDGE('',*,*,#6213,.T.);
#7941=ORIENTED_EDGE('',*,*,#6214,.T.);
#7942=ORIENTED_EDGE('',*,*,#6213,.F.);
#7943=ORIENTED_EDGE('',*,*,#6173,.T.);
#7944=ORIENTED_EDGE('',*,*,#6215,.T.);
#7945=ORIENTED_EDGE('',*,*,#6144,.T.);
#7946=ORIENTED_EDGE('',*,*,#6215,.F.);
#7947=ORIENTED_EDGE('',*,*,#6180,.T.);
#7948=ORIENTED_EDGE('',*,*,#6216,.T.);
#7949=ORIENTED_EDGE('',*,*,#6138,.T.);
#7950=ORIENTED_EDGE('',*,*,#6216,.F.);
#7951=ORIENTED_EDGE('',*,*,#6179,.T.);
#7952=ORIENTED_EDGE('',*,*,#6217,.T.);
#7953=ORIENTED_EDGE('',*,*,#6176,.T.);
#7954=ORIENTED_EDGE('',*,*,#6218,.T.);
#7955=ORIENTED_EDGE('',*,*,#6147,.T.);
#7956=ORIENTED_EDGE('',*,*,#6218,.F.);
#7957=ORIENTED_EDGE('',*,*,#6210,.T.);
#7958=ORIENTED_EDGE('',*,*,#6219,.T.);
#7959=ORIENTED_EDGE('',*,*,#6220,.F.);
#7960=ORIENTED_EDGE('',*,*,#6221,.F.);
#7961=ORIENTED_EDGE('',*,*,#6198,.T.);
#7962=ORIENTED_EDGE('',*,*,#6199,.T.);
#7963=ORIENTED_EDGE('',*,*,#6222,.T.);
#7964=ORIENTED_EDGE('',*,*,#6223,.T.);
#7965=ORIENTED_EDGE('',*,*,#6222,.F.);
#7966=ORIENTED_EDGE('',*,*,#6224,.F.);
#7967=ORIENTED_EDGE('',*,*,#6225,.T.);
#7968=ORIENTED_EDGE('',*,*,#6226,.F.);
#7969=ORIENTED_EDGE('',*,*,#6225,.F.);
#7970=ORIENTED_EDGE('',*,*,#6227,.F.);
#7971=ORIENTED_EDGE('',*,*,#6228,.T.);
#7972=ORIENTED_EDGE('',*,*,#6229,.F.);
#7973=ORIENTED_EDGE('',*,*,#6228,.F.);
#7974=ORIENTED_EDGE('',*,*,#6230,.F.);
#7975=ORIENTED_EDGE('',*,*,#6231,.T.);
#7976=ORIENTED_EDGE('',*,*,#6232,.F.);
#7977=ORIENTED_EDGE('',*,*,#6231,.F.);
#7978=ORIENTED_EDGE('',*,*,#6170,.T.);
#7979=ORIENTED_EDGE('',*,*,#6233,.T.);
#7980=ORIENTED_EDGE('',*,*,#6150,.T.);
#7981=ORIENTED_EDGE('',*,*,#6233,.F.);
#7982=ORIENTED_EDGE('',*,*,#6185,.T.);
#7983=ORIENTED_EDGE('',*,*,#6234,.T.);
#7984=ORIENTED_EDGE('',*,*,#6141,.T.);
#7985=ORIENTED_EDGE('',*,*,#6234,.F.);
#7986=ORIENTED_EDGE('',*,*,#6184,.T.);
#7987=ORIENTED_EDGE('',*,*,#6235,.T.);
#7988=ORIENTED_EDGE('',*,*,#6167,.T.);
#7989=ORIENTED_EDGE('',*,*,#6236,.T.);
#7990=ORIENTED_EDGE('',*,*,#6153,.T.);
#7991=ORIENTED_EDGE('',*,*,#6236,.F.);
#7992=ORIENTED_EDGE('',*,*,#6194,.T.);
#7993=ORIENTED_EDGE('',*,*,#6195,.T.);
#7994=ORIENTED_EDGE('',*,*,#6237,.T.);
#7995=ORIENTED_EDGE('',*,*,#6238,.F.);
#7996=ORIENTED_EDGE('',*,*,#6237,.F.);
#7997=ORIENTED_EDGE('',*,*,#6239,.T.);
#7998=ORIENTED_EDGE('',*,*,#6240,.T.);
#7999=ORIENTED_EDGE('',*,*,#6241,.T.);
#8000=ORIENTED_EDGE('',*,*,#6240,.F.);
#8001=ORIENTED_EDGE('',*,*,#6242,.T.);
#8002=ORIENTED_EDGE('',*,*,#6243,.T.);
#8003=ORIENTED_EDGE('',*,*,#6244,.T.);
#8004=ORIENTED_EDGE('',*,*,#6243,.F.);
#8005=ORIENTED_EDGE('',*,*,#6245,.T.);
#8006=ORIENTED_EDGE('',*,*,#6246,.T.);
#8007=ORIENTED_EDGE('',*,*,#6247,.T.);
#8008=ORIENTED_EDGE('',*,*,#6246,.F.);
#8009=ORIENTED_EDGE('',*,*,#6193,.T.);
#8010=ORIENTED_EDGE('',*,*,#6248,.T.);
#8011=ORIENTED_EDGE('',*,*,#6189,.T.);
#8012=ORIENTED_EDGE('',*,*,#6190,.T.);
#8013=ORIENTED_EDGE('',*,*,#6248,.F.);
#8014=ORIENTED_EDGE('',*,*,#6249,.F.);
#8015=ORIENTED_EDGE('',*,*,#6250,.T.);
#8016=ORIENTED_EDGE('',*,*,#6251,.F.);
#8017=ORIENTED_EDGE('',*,*,#6250,.F.);
#8018=ORIENTED_EDGE('',*,*,#6163,.T.);
#8019=ORIENTED_EDGE('',*,*,#6252,.T.);
#8020=ORIENTED_EDGE('',*,*,#6253,.T.);
#8021=ORIENTED_EDGE('',*,*,#6254,.F.);
#8022=ORIENTED_EDGE('',*,*,#6255,.T.);
#8023=ORIENTED_EDGE('',*,*,#6256,.T.);
#8024=ORIENTED_EDGE('',*,*,#6257,.T.);
#8025=ORIENTED_EDGE('',*,*,#6256,.F.);
#8026=ORIENTED_EDGE('',*,*,#6258,.F.);
#8027=ORIENTED_EDGE('',*,*,#6259,.T.);
#8028=ORIENTED_EDGE('',*,*,#6260,.T.);
#8029=ORIENTED_EDGE('',*,*,#6261,.T.);
#8030=ORIENTED_EDGE('',*,*,#6262,.F.);
#8031=ORIENTED_EDGE('',*,*,#6263,.T.);
#8032=ORIENTED_EDGE('',*,*,#6264,.T.);
#8033=ORIENTED_EDGE('',*,*,#6265,.F.);
#8034=ORIENTED_EDGE('',*,*,#6266,.T.);
#8035=ORIENTED_EDGE('',*,*,#6267,.T.);
#8036=ORIENTED_EDGE('',*,*,#6268,.T.);
#8037=ORIENTED_EDGE('',*,*,#6269,.F.);
#8038=ORIENTED_EDGE('',*,*,#6270,.F.);
#8039=ORIENTED_EDGE('',*,*,#6207,.T.);
#8040=ORIENTED_EDGE('',*,*,#6271,.F.);
#8041=ORIENTED_EDGE('',*,*,#6272,.T.);
#8042=ORIENTED_EDGE('',*,*,#6273,.T.);
#8043=ORIENTED_EDGE('',*,*,#6274,.T.);
#8044=ORIENTED_EDGE('',*,*,#6275,.T.);
#8045=ORIENTED_EDGE('',*,*,#6276,.T.);
#8046=ORIENTED_EDGE('',*,*,#6277,.T.);
#8047=ORIENTED_EDGE('',*,*,#6278,.F.);
#8048=ORIENTED_EDGE('',*,*,#6279,.T.);
#8049=ORIENTED_EDGE('',*,*,#6280,.T.);
#8050=ORIENTED_EDGE('',*,*,#6281,.T.);
#8051=ORIENTED_EDGE('',*,*,#6282,.F.);
#8052=ORIENTED_EDGE('',*,*,#6283,.T.);
#8053=ORIENTED_EDGE('',*,*,#6284,.T.);
#8054=ORIENTED_EDGE('',*,*,#6285,.F.);
#8055=ORIENTED_EDGE('',*,*,#6286,.T.);
#8056=ORIENTED_EDGE('',*,*,#6287,.F.);
#8057=ORIENTED_EDGE('',*,*,#6288,.F.);
#8058=ORIENTED_EDGE('',*,*,#6289,.F.);
#8059=ORIENTED_EDGE('',*,*,#6290,.F.);
#8060=ORIENTED_EDGE('',*,*,#6291,.F.);
#8061=ORIENTED_EDGE('',*,*,#6292,.T.);
#8062=ORIENTED_EDGE('',*,*,#6293,.T.);
#8063=ORIENTED_EDGE('',*,*,#6294,.T.);
#8064=ORIENTED_EDGE('',*,*,#6295,.T.);
#8065=ORIENTED_EDGE('',*,*,#6296,.T.);
#8066=ORIENTED_EDGE('',*,*,#6297,.T.);
#8067=ORIENTED_EDGE('',*,*,#6298,.T.);
#8068=ORIENTED_EDGE('',*,*,#6299,.F.);
#8069=ORIENTED_EDGE('',*,*,#6300,.T.);
#8070=ORIENTED_EDGE('',*,*,#6301,.T.);
#8071=ORIENTED_EDGE('',*,*,#6302,.T.);
#8072=ORIENTED_EDGE('',*,*,#6220,.T.);
#8073=ORIENTED_EDGE('',*,*,#6303,.T.);
#8074=ORIENTED_EDGE('',*,*,#6304,.F.);
#8075=ORIENTED_EDGE('',*,*,#6305,.F.);
#8076=ORIENTED_EDGE('',*,*,#6253,.F.);
#8077=ORIENTED_EDGE('',*,*,#6306,.F.);
#8078=ORIENTED_EDGE('',*,*,#6307,.F.);
#8079=ORIENTED_EDGE('',*,*,#6308,.T.);
#8080=ORIENTED_EDGE('',*,*,#6304,.T.);
#8081=ORIENTED_EDGE('',*,*,#6309,.T.);
#8082=ORIENTED_EDGE('',*,*,#6310,.F.);
#8083=ORIENTED_EDGE('',*,*,#6311,.F.);
#8084=ORIENTED_EDGE('',*,*,#6312,.F.);
#8085=ORIENTED_EDGE('',*,*,#6313,.T.);
#8086=ORIENTED_EDGE('',*,*,#6307,.T.);
#8087=ORIENTED_EDGE('',*,*,#6314,.F.);
#8088=ORIENTED_EDGE('',*,*,#6315,.T.);
#8089=ORIENTED_EDGE('',*,*,#6316,.T.);
#8090=ORIENTED_EDGE('',*,*,#6317,.F.);
#8091=ORIENTED_EDGE('',*,*,#6310,.T.);
#8092=ORIENTED_EDGE('',*,*,#6318,.F.);
#8093=ORIENTED_EDGE('',*,*,#6319,.T.);
#8094=ORIENTED_EDGE('',*,*,#6320,.T.);
#8095=ORIENTED_EDGE('',*,*,#6312,.T.);
#8096=ORIENTED_EDGE('',*,*,#6321,.F.);
#8097=ORIENTED_EDGE('',*,*,#6322,.T.);
#8098=ORIENTED_EDGE('',*,*,#6254,.T.);
#8099=ORIENTED_EDGE('',*,*,#6305,.T.);
#8100=ORIENTED_EDGE('',*,*,#6311,.T.);
#8101=ORIENTED_EDGE('',*,*,#6317,.T.);
#8102=ORIENTED_EDGE('',*,*,#6323,.T.);
#8103=ORIENTED_EDGE('',*,*,#6258,.T.);
#8104=ORIENTED_EDGE('',*,*,#6252,.F.);
#8105=ORIENTED_EDGE('',*,*,#6324,.T.);
#8106=ORIENTED_EDGE('',*,*,#6325,.T.);
#8107=ORIENTED_EDGE('',*,*,#6269,.T.);
#8108=ORIENTED_EDGE('',*,*,#6326,.T.);
#8109=ORIENTED_EDGE('',*,*,#6318,.T.);
#8110=ORIENTED_EDGE('',*,*,#6314,.T.);
#8111=ORIENTED_EDGE('',*,*,#6306,.T.);
#8112=ORIENTED_EDGE('',*,*,#6327,.T.);
#8113=ORIENTED_EDGE('',*,*,#6328,.T.);
#8114=ORIENTED_EDGE('',*,*,#6329,.T.);
#8115=ORIENTED_EDGE('',*,*,#6263,.F.);
#8116=ORIENTED_EDGE('',*,*,#6330,.T.);
#8117=ORIENTED_EDGE('',*,*,#6331,.F.);
#8118=ORIENTED_EDGE('',*,*,#6332,.T.);
#8119=ORIENTED_EDGE('',*,*,#6333,.F.);
#8120=ORIENTED_EDGE('',*,*,#6156,.T.);
#8121=ORIENTED_EDGE('',*,*,#6334,.T.);
#8122=ORIENTED_EDGE('',*,*,#6335,.T.);
#8123=ORIENTED_EDGE('',*,*,#6291,.T.);
#8124=ORIENTED_EDGE('',*,*,#6336,.F.);
#8125=ORIENTED_EDGE('',*,*,#6337,.T.);
#8126=ORIENTED_EDGE('',*,*,#6338,.F.);
#8127=ORIENTED_EDGE('',*,*,#6339,.T.);
#8128=ORIENTED_EDGE('',*,*,#6301,.F.);
#8129=ORIENTED_EDGE('',*,*,#6224,.T.);
#8130=ORIENTED_EDGE('',*,*,#6227,.T.);
#8131=ORIENTED_EDGE('',*,*,#6230,.T.);
#8132=ORIENTED_EDGE('',*,*,#6201,.T.);
#8133=ORIENTED_EDGE('',*,*,#6340,.F.);
#8134=ORIENTED_EDGE('',*,*,#6341,.T.);
#8135=ORIENTED_EDGE('',*,*,#6321,.T.);
#8136=ORIENTED_EDGE('',*,*,#6262,.T.);
#8137=ORIENTED_EDGE('',*,*,#6342,.T.);
#8138=ORIENTED_EDGE('',*,*,#6270,.T.);
#8139=ORIENTED_EDGE('',*,*,#6325,.F.);
#8140=ORIENTED_EDGE('',*,*,#6343,.T.);
#8141=ORIENTED_EDGE('',*,*,#6344,.F.);
#8142=ORIENTED_EDGE('',*,*,#6345,.T.);
#8143=ORIENTED_EDGE('',*,*,#6346,.T.);
#8144=ORIENTED_EDGE('',*,*,#6347,.T.);
#8145=ORIENTED_EDGE('',*,*,#6276,.F.);
#8146=ORIENTED_EDGE('',*,*,#6348,.T.);
#8147=ORIENTED_EDGE('',*,*,#6349,.F.);
#8148=ORIENTED_EDGE('',*,*,#6350,.T.);
#8149=ORIENTED_EDGE('',*,*,#6351,.F.);
#8150=ORIENTED_EDGE('',*,*,#6352,.T.);
#8151=ORIENTED_EDGE('',*,*,#6353,.T.);
#8152=ORIENTED_EDGE('',*,*,#6354,.T.);
#8153=ORIENTED_EDGE('',*,*,#6355,.T.);
#8154=ORIENTED_EDGE('',*,*,#6182,.T.);
#8155=ORIENTED_EDGE('',*,*,#6356,.T.);
#8156=ORIENTED_EDGE('',*,*,#6357,.F.);
#8157=ORIENTED_EDGE('',*,*,#6358,.T.);
#8158=ORIENTED_EDGE('',*,*,#6359,.F.);
#8159=ORIENTED_EDGE('',*,*,#6360,.T.);
#8160=ORIENTED_EDGE('',*,*,#6168,.T.);
#8161=ORIENTED_EDGE('',*,*,#6165,.T.);
#8162=ORIENTED_EDGE('',*,*,#6187,.T.);
#8163=ORIENTED_EDGE('',*,*,#6361,.F.);
#8164=ORIENTED_EDGE('',*,*,#6362,.T.);
#8165=ORIENTED_EDGE('',*,*,#6351,.T.);
#8166=ORIENTED_EDGE('',*,*,#6363,.T.);
#8167=ORIENTED_EDGE('',*,*,#6364,.F.);
#8168=ORIENTED_EDGE('',*,*,#6365,.T.);
#8169=ORIENTED_EDGE('',*,*,#6366,.T.);
#8170=ORIENTED_EDGE('',*,*,#6367,.F.);
#8171=ORIENTED_EDGE('',*,*,#6367,.T.);
#8172=ORIENTED_EDGE('',*,*,#6368,.T.);
#8173=ORIENTED_EDGE('',*,*,#6369,.F.);
#8174=ORIENTED_EDGE('',*,*,#6370,.F.);
#8175=ORIENTED_EDGE('',*,*,#6371,.T.);
#8176=ORIENTED_EDGE('',*,*,#6372,.T.);
#8177=ORIENTED_EDGE('',*,*,#6373,.T.);
#8178=ORIENTED_EDGE('',*,*,#6374,.T.);
#8179=ORIENTED_EDGE('',*,*,#6375,.T.);
#8180=ORIENTED_EDGE('',*,*,#6376,.T.);
#8181=ORIENTED_EDGE('',*,*,#6377,.T.);
#8182=ORIENTED_EDGE('',*,*,#6378,.T.);
#8183=ORIENTED_EDGE('',*,*,#6379,.T.);
#8184=ORIENTED_EDGE('',*,*,#6380,.T.);
#8185=ORIENTED_EDGE('',*,*,#6381,.T.);
#8186=ORIENTED_EDGE('',*,*,#6382,.T.);
#8187=ORIENTED_EDGE('',*,*,#6361,.T.);
#8188=ORIENTED_EDGE('',*,*,#6383,.T.);
#8189=ORIENTED_EDGE('',*,*,#6384,.T.);
#8190=ORIENTED_EDGE('',*,*,#6385,.T.);
#8191=ORIENTED_EDGE('',*,*,#6278,.T.);
#8192=ORIENTED_EDGE('',*,*,#6242,.F.);
#8193=ORIENTED_EDGE('',*,*,#6245,.F.);
#8194=ORIENTED_EDGE('',*,*,#6239,.F.);
#8195=ORIENTED_EDGE('',*,*,#6197,.T.);
#8196=ORIENTED_EDGE('',*,*,#6274,.F.);
#8197=ORIENTED_EDGE('',*,*,#6386,.F.);
#8198=ORIENTED_EDGE('',*,*,#6387,.T.);
#8199=ORIENTED_EDGE('',*,*,#6388,.T.);
#8200=ORIENTED_EDGE('',*,*,#6389,.T.);
#8201=ORIENTED_EDGE('',*,*,#6390,.T.);
#8202=ORIENTED_EDGE('',*,*,#6284,.F.);
#8203=ORIENTED_EDGE('',*,*,#6391,.F.);
#8204=ORIENTED_EDGE('',*,*,#6349,.T.);
#8205=ORIENTED_EDGE('',*,*,#6392,.T.);
#8206=ORIENTED_EDGE('',*,*,#6384,.F.);
#8207=ORIENTED_EDGE('',*,*,#6393,.T.);
#8208=ORIENTED_EDGE('',*,*,#6374,.F.);
#8209=ORIENTED_EDGE('',*,*,#6394,.T.);
#8210=ORIENTED_EDGE('',*,*,#6344,.T.);
#8211=ORIENTED_EDGE('',*,*,#6395,.T.);
#8212=ORIENTED_EDGE('',*,*,#6376,.F.);
#8213=ORIENTED_EDGE('',*,*,#6396,.T.);
#8214=ORIENTED_EDGE('',*,*,#6359,.T.);
#8215=ORIENTED_EDGE('',*,*,#6397,.T.);
#8216=ORIENTED_EDGE('',*,*,#6378,.F.);
#8217=ORIENTED_EDGE('',*,*,#6398,.T.);
#8218=ORIENTED_EDGE('',*,*,#6357,.T.);
#8219=ORIENTED_EDGE('',*,*,#6399,.T.);
#8220=ORIENTED_EDGE('',*,*,#6238,.T.);
#8221=ORIENTED_EDGE('',*,*,#6214,.F.);
#8222=ORIENTED_EDGE('',*,*,#6400,.F.);
#8223=ORIENTED_EDGE('',*,*,#6401,.T.);
#8224=ORIENTED_EDGE('',*,*,#6386,.T.);
#8225=ORIENTED_EDGE('',*,*,#6273,.F.);
#8226=ORIENTED_EDGE('',*,*,#6402,.T.);
#8227=ORIENTED_EDGE('',*,*,#6364,.T.);
#8228=ORIENTED_EDGE('',*,*,#6370,.T.);
#8229=ORIENTED_EDGE('',*,*,#6403,.T.);
#8230=ORIENTED_EDGE('',*,*,#6404,.F.);
#8231=ORIENTED_EDGE('',*,*,#6405,.T.);
#8232=ORIENTED_EDGE('',*,*,#6400,.T.);
#8233=ORIENTED_EDGE('',*,*,#6406,.T.);
#8234=ORIENTED_EDGE('',*,*,#6390,.F.);
#8235=ORIENTED_EDGE('',*,*,#6407,.T.);
#8236=ORIENTED_EDGE('',*,*,#6404,.T.);
#8237=ORIENTED_EDGE('',*,*,#6408,.T.);
#8238=ORIENTED_EDGE('',*,*,#6409,.T.);
#8239=ORIENTED_EDGE('',*,*,#6410,.T.);
#8240=ORIENTED_EDGE('',*,*,#6411,.T.);
#8241=ORIENTED_EDGE('',*,*,#6280,.F.);
#8242=ORIENTED_EDGE('',*,*,#6412,.T.);
#8243=ORIENTED_EDGE('',*,*,#6413,.T.);
#8244=ORIENTED_EDGE('',*,*,#6388,.F.);
#8245=ORIENTED_EDGE('',*,*,#6414,.T.);
#8246=ORIENTED_EDGE('',*,*,#6249,.T.);
#8247=ORIENTED_EDGE('',*,*,#6415,.T.);
#8248=ORIENTED_EDGE('',*,*,#6416,.T.);
#8249=ORIENTED_EDGE('',*,*,#6410,.F.);
#8250=ORIENTED_EDGE('',*,*,#6417,.F.);
#8251=ORIENTED_EDGE('',*,*,#6418,.F.);
#8252=ORIENTED_EDGE('',*,*,#6419,.T.);
#8253=ORIENTED_EDGE('',*,*,#6417,.T.);
#8254=ORIENTED_EDGE('',*,*,#6409,.F.);
#8255=ORIENTED_EDGE('',*,*,#6369,.T.);
#8256=ORIENTED_EDGE('',*,*,#6420,.T.);
#8257=ORIENTED_EDGE('',*,*,#6421,.T.);
#8258=ORIENTED_EDGE('',*,*,#6422,.T.);
#8259=ORIENTED_EDGE('',*,*,#6418,.T.);
#8260=ORIENTED_EDGE('',*,*,#6408,.F.);
#8261=ORIENTED_EDGE('',*,*,#6406,.F.);
#8262=ORIENTED_EDGE('',*,*,#6403,.F.);
#8263=ORIENTED_EDGE('',*,*,#6423,.T.);
#8264=ORIENTED_EDGE('',*,*,#6424,.T.);
#8265=ORIENTED_EDGE('',*,*,#6425,.T.);
#8266=ORIENTED_EDGE('',*,*,#6426,.T.);
#8267=ORIENTED_EDGE('',*,*,#6251,.T.);
#8268=ORIENTED_EDGE('',*,*,#6366,.F.);
#8269=ORIENTED_EDGE('',*,*,#6427,.T.);
#8270=ORIENTED_EDGE('',*,*,#6271,.T.);
#8271=ORIENTED_EDGE('',*,*,#6428,.T.);
#8272=ORIENTED_EDGE('',*,*,#6429,.T.);
#8273=ORIENTED_EDGE('',*,*,#6430,.T.);
#8274=ORIENTED_EDGE('',*,*,#6420,.F.);
#8275=ORIENTED_EDGE('',*,*,#6368,.F.);
#8276=ORIENTED_EDGE('',*,*,#6430,.F.);
#8277=ORIENTED_EDGE('',*,*,#6431,.T.);
#8278=ORIENTED_EDGE('',*,*,#6432,.T.);
#8279=ORIENTED_EDGE('',*,*,#6421,.F.);
#8280=ORIENTED_EDGE('',*,*,#6282,.T.);
#8281=ORIENTED_EDGE('',*,*,#6433,.T.);
#8282=ORIENTED_EDGE('',*,*,#6415,.F.);
#8283=ORIENTED_EDGE('',*,*,#6419,.F.);
#8284=ORIENTED_EDGE('',*,*,#6422,.F.);
#8285=ORIENTED_EDGE('',*,*,#6432,.F.);
#8286=ORIENTED_EDGE('',*,*,#6434,.T.);
#8287=ORIENTED_EDGE('',*,*,#6435,.T.);
#8288=ORIENTED_EDGE('',*,*,#6436,.T.);
#8289=ORIENTED_EDGE('',*,*,#6437,.T.);
#8290=ORIENTED_EDGE('',*,*,#6438,.T.);
#8291=ORIENTED_EDGE('',*,*,#6439,.T.);
#8292=ORIENTED_EDGE('',*,*,#6355,.F.);
#8293=ORIENTED_EDGE('',*,*,#6440,.T.);
#8294=ORIENTED_EDGE('',*,*,#6441,.T.);
#8295=ORIENTED_EDGE('',*,*,#6442,.T.);
#8296=ORIENTED_EDGE('',*,*,#6379,.F.);
#8297=ORIENTED_EDGE('',*,*,#6399,.F.);
#8298=ORIENTED_EDGE('',*,*,#6356,.F.);
#8299=ORIENTED_EDGE('',*,*,#6443,.F.);
#8300=ORIENTED_EDGE('',*,*,#6375,.F.);
#8301=ORIENTED_EDGE('',*,*,#6395,.F.);
#8302=ORIENTED_EDGE('',*,*,#6360,.F.);
#8303=ORIENTED_EDGE('',*,*,#6396,.F.);
#8304=ORIENTED_EDGE('',*,*,#6377,.F.);
#8305=ORIENTED_EDGE('',*,*,#6397,.F.);
#8306=ORIENTED_EDGE('',*,*,#6358,.F.);
#8307=ORIENTED_EDGE('',*,*,#6398,.F.);
#8308=ORIENTED_EDGE('',*,*,#6385,.F.);
#8309=ORIENTED_EDGE('',*,*,#6392,.F.);
#8310=ORIENTED_EDGE('',*,*,#6348,.F.);
#8311=ORIENTED_EDGE('',*,*,#6279,.F.);
#8312=ORIENTED_EDGE('',*,*,#6383,.F.);
#8313=ORIENTED_EDGE('',*,*,#6363,.F.);
#8314=ORIENTED_EDGE('',*,*,#6350,.F.);
#8315=ORIENTED_EDGE('',*,*,#6393,.F.);
#8316=ORIENTED_EDGE('',*,*,#6444,.F.);
#8317=ORIENTED_EDGE('',*,*,#6445,.T.);
#8318=ORIENTED_EDGE('',*,*,#6446,.T.);
#8319=ORIENTED_EDGE('',*,*,#6447,.T.);
#8320=ORIENTED_EDGE('',*,*,#6448,.F.);
#8321=ORIENTED_EDGE('',*,*,#6449,.T.);
#8322=ORIENTED_EDGE('',*,*,#6450,.F.);
#8323=ORIENTED_EDGE('',*,*,#6451,.T.);
#8324=ORIENTED_EDGE('',*,*,#6446,.F.);
#8325=ORIENTED_EDGE('',*,*,#6452,.T.);
#8326=ORIENTED_EDGE('',*,*,#6453,.F.);
#8327=ORIENTED_EDGE('',*,*,#6381,.F.);
#8328=ORIENTED_EDGE('',*,*,#6454,.T.);
#8329=ORIENTED_EDGE('',*,*,#6448,.T.);
#8330=ORIENTED_EDGE('',*,*,#6455,.T.);
#8331=ORIENTED_EDGE('',*,*,#6456,.T.);
#8332=ORIENTED_EDGE('',*,*,#6457,.T.);
#8333=ORIENTED_EDGE('',*,*,#6458,.T.);
#8334=ORIENTED_EDGE('',*,*,#6459,.F.);
#8335=ORIENTED_EDGE('',*,*,#6460,.F.);
#8336=ORIENTED_EDGE('',*,*,#6461,.T.);
#8337=ORIENTED_EDGE('',*,*,#6450,.T.);
#8338=ORIENTED_EDGE('',*,*,#6462,.T.);
#8339=ORIENTED_EDGE('',*,*,#6441,.F.);
#8340=ORIENTED_EDGE('',*,*,#6463,.T.);
#8341=ORIENTED_EDGE('',*,*,#6456,.F.);
#8342=ORIENTED_EDGE('',*,*,#6459,.T.);
#8343=ORIENTED_EDGE('',*,*,#6464,.T.);
#8344=ORIENTED_EDGE('',*,*,#6465,.T.);
#8345=ORIENTED_EDGE('',*,*,#6453,.T.);
#8346=ORIENTED_EDGE('',*,*,#6466,.T.);
#8347=ORIENTED_EDGE('',*,*,#6444,.T.);
#8348=ORIENTED_EDGE('',*,*,#6467,.T.);
#8349=ORIENTED_EDGE('',*,*,#6460,.T.);
#8350=ORIENTED_EDGE('',*,*,#6155,.T.);
#8351=ORIENTED_EDGE('',*,*,#6244,.F.);
#8352=ORIENTED_EDGE('',*,*,#6143,.T.);
#8353=ORIENTED_EDGE('',*,*,#6247,.F.);
#8354=ORIENTED_EDGE('',*,*,#6152,.T.);
#8355=ORIENTED_EDGE('',*,*,#6241,.F.);
#8356=ORIENTED_EDGE('',*,*,#6331,.T.);
#8357=ORIENTED_EDGE('',*,*,#6468,.T.);
#8358=ORIENTED_EDGE('',*,*,#6469,.F.);
#8359=ORIENTED_EDGE('',*,*,#6470,.T.);
#8360=ORIENTED_EDGE('',*,*,#6471,.F.);
#8361=ORIENTED_EDGE('',*,*,#6157,.T.);
#8362=ORIENTED_EDGE('',*,*,#6333,.T.);
#8363=ORIENTED_EDGE('',*,*,#6472,.T.);
#8364=ORIENTED_EDGE('',*,*,#6473,.F.);
#8365=ORIENTED_EDGE('',*,*,#6474,.T.);
#8366=ORIENTED_EDGE('',*,*,#6336,.T.);
#8367=ORIENTED_EDGE('',*,*,#6290,.T.);
#8368=ORIENTED_EDGE('',*,*,#6475,.F.);
#8369=ORIENTED_EDGE('',*,*,#6476,.T.);
#8370=ORIENTED_EDGE('',*,*,#6338,.T.);
#8371=ORIENTED_EDGE('',*,*,#6477,.T.);
#8372=ORIENTED_EDGE('',*,*,#6265,.T.);
#8373=ORIENTED_EDGE('',*,*,#6478,.T.);
#8374=ORIENTED_EDGE('',*,*,#6479,.T.);
#8375=ORIENTED_EDGE('',*,*,#6480,.T.);
#8376=ORIENTED_EDGE('',*,*,#6299,.T.);
#8377=ORIENTED_EDGE('',*,*,#6481,.T.);
#8378=ORIENTED_EDGE('',*,*,#6475,.T.);
#8379=ORIENTED_EDGE('',*,*,#6482,.T.);
#8380=ORIENTED_EDGE('',*,*,#6473,.T.);
#8381=ORIENTED_EDGE('',*,*,#6289,.T.);
#8382=ORIENTED_EDGE('',*,*,#6177,.T.);
#8383=ORIENTED_EDGE('',*,*,#6287,.T.);
#8384=ORIENTED_EDGE('',*,*,#6483,.T.);
#8385=ORIENTED_EDGE('',*,*,#6484,.T.);
#8386=ORIENTED_EDGE('',*,*,#6158,.T.);
#8387=ORIENTED_EDGE('',*,*,#6471,.T.);
#8388=ORIENTED_EDGE('',*,*,#6485,.T.);
#8389=ORIENTED_EDGE('',*,*,#6469,.T.);
#8390=ORIENTED_EDGE('',*,*,#6486,.T.);
#8391=ORIENTED_EDGE('',*,*,#6174,.T.);
#8392=ORIENTED_EDGE('',*,*,#6171,.T.);
#8393=ORIENTED_EDGE('',*,*,#6191,.T.);
#8394=ORIENTED_EDGE('',*,*,#6223,.F.);
#8395=ORIENTED_EDGE('',*,*,#6212,.F.);
#8396=ORIENTED_EDGE('',*,*,#6340,.T.);
#8397=ORIENTED_EDGE('',*,*,#6487,.T.);
#8398=ORIENTED_EDGE('',*,*,#6161,.T.);
#8399=ORIENTED_EDGE('',*,*,#6488,.T.);
#8400=ORIENTED_EDGE('',*,*,#6255,.F.);
#8401=ORIENTED_EDGE('',*,*,#6489,.F.);
#8402=ORIENTED_EDGE('',*,*,#6203,.T.);
#8403=ORIENTED_EDGE('',*,*,#6490,.F.);
#8404=ORIENTED_EDGE('',*,*,#6491,.T.);
#8405=ORIENTED_EDGE('',*,*,#6492,.T.);
#8406=ORIENTED_EDGE('',*,*,#6260,.F.);
#8407=ORIENTED_EDGE('',*,*,#6493,.T.);
#8408=ORIENTED_EDGE('',*,*,#6315,.F.);
#8409=ORIENTED_EDGE('',*,*,#6309,.F.);
#8410=ORIENTED_EDGE('',*,*,#6303,.F.);
#8411=ORIENTED_EDGE('',*,*,#6219,.F.);
#8412=ORIENTED_EDGE('',*,*,#6494,.T.);
#8413=ORIENTED_EDGE('',*,*,#6495,.T.);
#8414=ORIENTED_EDGE('',*,*,#6320,.F.);
#8415=ORIENTED_EDGE('',*,*,#6496,.T.);
#8416=ORIENTED_EDGE('',*,*,#6267,.F.);
#8417=ORIENTED_EDGE('',*,*,#6206,.T.);
#8418=ORIENTED_EDGE('',*,*,#6497,.T.);
#8419=ORIENTED_EDGE('',*,*,#6221,.T.);
#8420=ORIENTED_EDGE('',*,*,#6308,.F.);
#8421=ORIENTED_EDGE('',*,*,#6313,.F.);
#8422=ORIENTED_EDGE('',*,*,#6498,.T.);
#8423=ORIENTED_EDGE('',*,*,#6204,.T.);
#8424=ORIENTED_EDGE('',*,*,#6489,.T.);
#8425=ORIENTED_EDGE('',*,*,#6499,.T.);
#8426=ORIENTED_EDGE('',*,*,#6208,.T.);
#8427=ORIENTED_EDGE('',*,*,#6257,.F.);
#8428=ORIENTED_EDGE('',*,*,#6339,.F.);
#8429=ORIENTED_EDGE('',*,*,#6476,.F.);
#8430=ORIENTED_EDGE('',*,*,#6481,.F.);
#8431=ORIENTED_EDGE('',*,*,#6302,.F.);
#8432=ORIENTED_EDGE('',*,*,#6337,.F.);
#8433=ORIENTED_EDGE('',*,*,#6474,.F.);
#8434=ORIENTED_EDGE('',*,*,#6482,.F.);
#8435=ORIENTED_EDGE('',*,*,#6477,.F.);
#8436=ORIENTED_EDGE('',*,*,#6330,.F.);
#8437=ORIENTED_EDGE('',*,*,#6266,.F.);
#8438=ORIENTED_EDGE('',*,*,#6486,.F.);
#8439=ORIENTED_EDGE('',*,*,#6468,.F.);
#8440=ORIENTED_EDGE('',*,*,#6332,.F.);
#8441=ORIENTED_EDGE('',*,*,#6470,.F.);
#8442=ORIENTED_EDGE('',*,*,#6485,.F.);
#8443=ORIENTED_EDGE('',*,*,#6472,.F.);
#8444=ORIENTED_EDGE('',*,*,#6500,.T.);
#8445=ORIENTED_EDGE('',*,*,#6501,.T.);
#8446=ORIENTED_EDGE('',*,*,#6502,.F.);
#8447=ORIENTED_EDGE('',*,*,#6503,.T.);
#8448=ORIENTED_EDGE('',*,*,#6293,.F.);
#8449=ORIENTED_EDGE('',*,*,#6504,.T.);
#8450=ORIENTED_EDGE('',*,*,#6505,.T.);
#8451=ORIENTED_EDGE('',*,*,#6502,.T.);
#8452=ORIENTED_EDGE('',*,*,#6506,.T.);
#8453=ORIENTED_EDGE('',*,*,#6285,.T.);
#8454=ORIENTED_EDGE('',*,*,#6507,.T.);
#8455=ORIENTED_EDGE('',*,*,#6297,.F.);
#8456=ORIENTED_EDGE('',*,*,#6508,.T.);
#8457=ORIENTED_EDGE('',*,*,#6509,.T.);
#8458=ORIENTED_EDGE('',*,*,#6510,.T.);
#8459=ORIENTED_EDGE('',*,*,#6511,.T.);
#8460=ORIENTED_EDGE('',*,*,#6512,.T.);
#8461=ORIENTED_EDGE('',*,*,#6295,.F.);
#8462=ORIENTED_EDGE('',*,*,#6513,.T.);
#8463=ORIENTED_EDGE('',*,*,#6334,.F.);
#8464=ORIENTED_EDGE('',*,*,#6160,.F.);
#8465=ORIENTED_EDGE('',*,*,#6514,.T.);
#8466=ORIENTED_EDGE('',*,*,#6503,.F.);
#8467=ORIENTED_EDGE('',*,*,#6505,.F.);
#8468=ORIENTED_EDGE('',*,*,#6515,.T.);
#8469=ORIENTED_EDGE('',*,*,#6509,.F.);
#8470=ORIENTED_EDGE('',*,*,#6516,.T.);
#8471=ORIENTED_EDGE('',*,*,#6511,.F.);
#8472=ORIENTED_EDGE('',*,*,#6149,.T.);
#8473=ORIENTED_EDGE('',*,*,#6229,.T.);
#8474=ORIENTED_EDGE('',*,*,#6140,.T.);
#8475=ORIENTED_EDGE('',*,*,#6232,.T.);
#8476=ORIENTED_EDGE('',*,*,#6146,.T.);
#8477=ORIENTED_EDGE('',*,*,#6226,.T.);
#8478=ORIENTED_EDGE('',*,*,#6391,.T.);
#8479=ORIENTED_EDGE('',*,*,#6517,.T.);
#8480=ORIENTED_EDGE('',*,*,#6436,.F.);
#8481=ORIENTED_EDGE('',*,*,#6518,.T.);
#8482=ORIENTED_EDGE('',*,*,#6519,.F.);
#8483=ORIENTED_EDGE('',*,*,#6520,.T.);
#8484=ORIENTED_EDGE('',*,*,#6521,.T.);
#8485=ORIENTED_EDGE('',*,*,#6522,.T.);
#8486=ORIENTED_EDGE('',*,*,#6490,.T.);
#8487=ORIENTED_EDGE('',*,*,#6202,.T.);
#8488=ORIENTED_EDGE('',*,*,#6342,.F.);
#8489=ORIENTED_EDGE('',*,*,#6523,.T.);
#8490=ORIENTED_EDGE('',*,*,#6524,.F.);
#8491=ORIENTED_EDGE('',*,*,#6525,.T.);
#8492=ORIENTED_EDGE('',*,*,#6526,.T.);
#8493=ORIENTED_EDGE('',*,*,#6527,.T.);
#8494=ORIENTED_EDGE('',*,*,#6526,.F.);
#8495=ORIENTED_EDGE('',*,*,#6528,.T.);
#8496=ORIENTED_EDGE('',*,*,#6529,.T.);
#8497=ORIENTED_EDGE('',*,*,#6530,.T.);
#8498=ORIENTED_EDGE('',*,*,#6521,.F.);
#8499=ORIENTED_EDGE('',*,*,#6531,.T.);
#8500=ORIENTED_EDGE('',*,*,#6532,.T.);
#8501=ORIENTED_EDGE('',*,*,#6533,.T.);
#8502=ORIENTED_EDGE('',*,*,#6534,.T.);
#8503=ORIENTED_EDGE('',*,*,#6535,.T.);
#8504=ORIENTED_EDGE('',*,*,#6524,.T.);
#8505=ORIENTED_EDGE('',*,*,#6536,.T.);
#8506=ORIENTED_EDGE('',*,*,#6537,.T.);
#8507=ORIENTED_EDGE('',*,*,#6538,.T.);
#8508=ORIENTED_EDGE('',*,*,#6519,.T.);
#8509=ORIENTED_EDGE('',*,*,#6539,.T.);
#8510=ORIENTED_EDGE('',*,*,#6516,.F.);
#8511=ORIENTED_EDGE('',*,*,#6508,.F.);
#8512=ORIENTED_EDGE('',*,*,#6296,.F.);
#8513=ORIENTED_EDGE('',*,*,#6512,.F.);
#8514=ORIENTED_EDGE('',*,*,#6515,.F.);
#8515=ORIENTED_EDGE('',*,*,#6504,.F.);
#8516=ORIENTED_EDGE('',*,*,#6298,.F.);
#8517=ORIENTED_EDGE('',*,*,#6510,.F.);
#8518=ORIENTED_EDGE('',*,*,#6466,.F.);
#8519=ORIENTED_EDGE('',*,*,#6455,.F.);
#8520=ORIENTED_EDGE('',*,*,#6452,.F.);
#8521=ORIENTED_EDGE('',*,*,#6445,.F.);
#8522=ORIENTED_EDGE('',*,*,#6467,.F.);
#8523=ORIENTED_EDGE('',*,*,#6447,.F.);
#8524=ORIENTED_EDGE('',*,*,#6451,.F.);
#8525=ORIENTED_EDGE('',*,*,#6461,.F.);
#8526=ORIENTED_EDGE('',*,*,#6261,.F.);
#8527=ORIENTED_EDGE('',*,*,#6495,.F.);
#8528=ORIENTED_EDGE('',*,*,#6540,.F.);
#8529=ORIENTED_EDGE('',*,*,#6491,.F.);
#8530=ORIENTED_EDGE('',*,*,#6523,.F.);
#8531=ORIENTED_EDGE('',*,*,#6540,.T.);
#8532=ORIENTED_EDGE('',*,*,#6494,.F.);
#8533=ORIENTED_EDGE('',*,*,#6209,.F.);
#8534=ORIENTED_EDGE('',*,*,#6499,.F.);
#8535=ORIENTED_EDGE('',*,*,#6492,.F.);
#8536=ORIENTED_EDGE('',*,*,#6211,.T.);
#8537=ORIENTED_EDGE('',*,*,#6497,.F.);
#8538=ORIENTED_EDGE('',*,*,#6205,.F.);
#8539=ORIENTED_EDGE('',*,*,#6498,.F.);
#8540=ORIENTED_EDGE('',*,*,#6518,.F.);
#8541=ORIENTED_EDGE('',*,*,#6439,.F.);
#8542=ORIENTED_EDGE('',*,*,#6541,.F.);
#8543=ORIENTED_EDGE('',*,*,#6428,.F.);
#8544=ORIENTED_EDGE('',*,*,#6275,.F.);
#8545=ORIENTED_EDGE('',*,*,#6283,.F.);
#8546=ORIENTED_EDGE('',*,*,#6435,.F.);
#8547=ORIENTED_EDGE('',*,*,#6542,.F.);
#8548=ORIENTED_EDGE('',*,*,#6437,.F.);
#8549=ORIENTED_EDGE('',*,*,#6517,.F.);
#8550=ORIENTED_EDGE('',*,*,#6543,.F.);
#8551=ORIENTED_EDGE('',*,*,#6438,.F.);
#8552=ORIENTED_EDGE('',*,*,#6544,.F.);
#8553=ORIENTED_EDGE('',*,*,#6426,.F.);
#8554=ORIENTED_EDGE('',*,*,#6541,.T.);
#8555=ORIENTED_EDGE('',*,*,#6543,.T.);
#8556=ORIENTED_EDGE('',*,*,#6545,.F.);
#8557=ORIENTED_EDGE('',*,*,#6544,.T.);
#8558=ORIENTED_EDGE('',*,*,#6542,.T.);
#8559=ORIENTED_EDGE('',*,*,#6546,.F.);
#8560=ORIENTED_EDGE('',*,*,#6545,.T.);
#8561=ORIENTED_EDGE('',*,*,#6425,.F.);
#8562=ORIENTED_EDGE('',*,*,#6547,.F.);
#8563=ORIENTED_EDGE('',*,*,#6429,.F.);
#8564=ORIENTED_EDGE('',*,*,#6546,.T.);
#8565=ORIENTED_EDGE('',*,*,#6434,.F.);
#8566=ORIENTED_EDGE('',*,*,#6548,.F.);
#8567=ORIENTED_EDGE('',*,*,#6423,.F.);
#8568=ORIENTED_EDGE('',*,*,#6547,.T.);
#8569=ORIENTED_EDGE('',*,*,#6424,.F.);
#8570=ORIENTED_EDGE('',*,*,#6548,.T.);
#8571=ORIENTED_EDGE('',*,*,#6431,.F.);
#8572=ORIENTED_EDGE('',*,*,#6500,.F.);
#8573=ORIENTED_EDGE('',*,*,#6514,.F.);
#8574=ORIENTED_EDGE('',*,*,#6159,.T.);
#8575=ORIENTED_EDGE('',*,*,#6484,.F.);
#8576=ORIENTED_EDGE('',*,*,#6549,.T.);
#8577=ORIENTED_EDGE('',*,*,#6458,.F.);
#8578=ORIENTED_EDGE('',*,*,#6550,.T.);
#8579=ORIENTED_EDGE('',*,*,#6353,.F.);
#8580=ORIENTED_EDGE('',*,*,#6551,.T.);
#8581=ORIENTED_EDGE('',*,*,#6464,.F.);
#8582=ORIENTED_EDGE('',*,*,#6531,.F.);
#8583=ORIENTED_EDGE('',*,*,#6520,.F.);
#8584=ORIENTED_EDGE('',*,*,#6538,.F.);
#8585=ORIENTED_EDGE('',*,*,#6552,.T.);
#8586=ORIENTED_EDGE('',*,*,#6479,.F.);
#8587=ORIENTED_EDGE('',*,*,#6553,.T.);
#8588=ORIENTED_EDGE('',*,*,#6530,.F.);
#8589=ORIENTED_EDGE('',*,*,#6554,.T.);
#8590=ORIENTED_EDGE('',*,*,#6346,.F.);
#8591=ORIENTED_EDGE('',*,*,#6555,.T.);
#8592=ORIENTED_EDGE('',*,*,#6539,.F.);
#8593=ORIENTED_EDGE('',*,*,#6522,.F.);
#8594=ORIENTED_EDGE('',*,*,#6323,.F.);
#8595=ORIENTED_EDGE('',*,*,#6316,.F.);
#8596=ORIENTED_EDGE('',*,*,#6493,.F.);
#8597=ORIENTED_EDGE('',*,*,#6259,.F.);
#8598=ORIENTED_EDGE('',*,*,#6496,.F.);
#8599=ORIENTED_EDGE('',*,*,#6319,.F.);
#8600=ORIENTED_EDGE('',*,*,#6326,.F.);
#8601=ORIENTED_EDGE('',*,*,#6268,.F.);
#8602=ORIENTED_EDGE('',*,*,#6462,.F.);
#8603=ORIENTED_EDGE('',*,*,#6449,.F.);
#8604=ORIENTED_EDGE('',*,*,#6454,.F.);
#8605=ORIENTED_EDGE('',*,*,#6380,.F.);
#8606=ORIENTED_EDGE('',*,*,#6442,.F.);
#8607=ORIENTED_EDGE('',*,*,#6292,.F.);
#8608=ORIENTED_EDGE('',*,*,#6335,.F.);
#8609=ORIENTED_EDGE('',*,*,#6513,.F.);
#8610=ORIENTED_EDGE('',*,*,#6294,.F.);
#8611=ORIENTED_EDGE('',*,*,#6507,.F.);
#8612=ORIENTED_EDGE('',*,*,#6433,.F.);
#8613=ORIENTED_EDGE('',*,*,#6281,.F.);
#8614=ORIENTED_EDGE('',*,*,#6411,.F.);
#8615=ORIENTED_EDGE('',*,*,#6416,.F.);
#8616=ORIENTED_EDGE('',*,*,#6402,.F.);
#8617=ORIENTED_EDGE('',*,*,#6272,.F.);
#8618=ORIENTED_EDGE('',*,*,#6427,.F.);
#8619=ORIENTED_EDGE('',*,*,#6365,.F.);
#8620=ORIENTED_EDGE('',*,*,#6183,.T.);
#8621=ORIENTED_EDGE('',*,*,#6443,.T.);
#8622=ORIENTED_EDGE('',*,*,#6186,.T.);
#8623=ORIENTED_EDGE('',*,*,#6235,.F.);
#8624=ORIENTED_EDGE('',*,*,#6181,.T.);
#8625=ORIENTED_EDGE('',*,*,#6217,.F.);
#8626=ORIENTED_EDGE('',*,*,#6178,.T.);
#8627=ORIENTED_EDGE('',*,*,#6288,.T.);
#8628=ORIENTED_EDGE('',*,*,#6341,.F.);
#8629=ORIENTED_EDGE('',*,*,#6488,.F.);
#8630=ORIENTED_EDGE('',*,*,#6164,.F.);
#8631=ORIENTED_EDGE('',*,*,#6322,.F.);
#8632=ORIENTED_EDGE('',*,*,#6343,.F.);
#8633=ORIENTED_EDGE('',*,*,#6324,.F.);
#8634=ORIENTED_EDGE('',*,*,#6162,.T.);
#8635=ORIENTED_EDGE('',*,*,#6487,.F.);
#8636=ORIENTED_EDGE('',*,*,#6387,.F.);
#8637=ORIENTED_EDGE('',*,*,#6401,.F.);
#8638=ORIENTED_EDGE('',*,*,#6556,.F.);
#8639=ORIENTED_EDGE('',*,*,#6414,.F.);
#8640=ORIENTED_EDGE('',*,*,#6556,.T.);
#8641=ORIENTED_EDGE('',*,*,#6405,.F.);
#8642=ORIENTED_EDGE('',*,*,#6557,.F.);
#8643=ORIENTED_EDGE('',*,*,#6412,.F.);
#8644=ORIENTED_EDGE('',*,*,#6389,.F.);
#8645=ORIENTED_EDGE('',*,*,#6413,.F.);
#8646=ORIENTED_EDGE('',*,*,#6557,.T.);
#8647=ORIENTED_EDGE('',*,*,#6407,.F.);
#8648=ORIENTED_EDGE('',*,*,#6529,.F.);
#8649=ORIENTED_EDGE('',*,*,#6558,.T.);
#8650=ORIENTED_EDGE('',*,*,#6371,.F.);
#8651=ORIENTED_EDGE('',*,*,#6277,.F.);
#8652=ORIENTED_EDGE('',*,*,#6347,.F.);
#8653=ORIENTED_EDGE('',*,*,#6554,.F.);
#8654=ORIENTED_EDGE('',*,*,#6329,.F.);
#8655=ORIENTED_EDGE('',*,*,#6559,.T.);
#8656=ORIENTED_EDGE('',*,*,#6532,.F.);
#8657=ORIENTED_EDGE('',*,*,#6553,.F.);
#8658=ORIENTED_EDGE('',*,*,#6478,.F.);
#8659=ORIENTED_EDGE('',*,*,#6264,.F.);
#8660=ORIENTED_EDGE('',*,*,#6537,.F.);
#8661=ORIENTED_EDGE('',*,*,#6560,.T.);
#8662=ORIENTED_EDGE('',*,*,#6327,.F.);
#8663=ORIENTED_EDGE('',*,*,#6300,.F.);
#8664=ORIENTED_EDGE('',*,*,#6480,.F.);
#8665=ORIENTED_EDGE('',*,*,#6552,.F.);
#8666=ORIENTED_EDGE('',*,*,#6373,.F.);
#8667=ORIENTED_EDGE('',*,*,#6561,.T.);
#8668=ORIENTED_EDGE('',*,*,#6534,.F.);
#8669=ORIENTED_EDGE('',*,*,#6555,.F.);
#8670=ORIENTED_EDGE('',*,*,#6345,.F.);
#8671=ORIENTED_EDGE('',*,*,#6394,.F.);
#8672=ORIENTED_EDGE('',*,*,#6352,.F.);
#8673=ORIENTED_EDGE('',*,*,#6362,.F.);
#8674=ORIENTED_EDGE('',*,*,#6382,.F.);
#8675=ORIENTED_EDGE('',*,*,#6465,.F.);
#8676=ORIENTED_EDGE('',*,*,#6551,.F.);
#8677=ORIENTED_EDGE('',*,*,#6506,.F.);
#8678=ORIENTED_EDGE('',*,*,#6501,.F.);
#8679=ORIENTED_EDGE('',*,*,#6549,.F.);
#8680=ORIENTED_EDGE('',*,*,#6483,.F.);
#8681=ORIENTED_EDGE('',*,*,#6286,.F.);
#8682=ORIENTED_EDGE('',*,*,#6463,.F.);
#8683=ORIENTED_EDGE('',*,*,#6440,.F.);
#8684=ORIENTED_EDGE('',*,*,#6354,.F.);
#8685=ORIENTED_EDGE('',*,*,#6550,.F.);
#8686=ORIENTED_EDGE('',*,*,#6457,.F.);
#8687=ORIENTED_EDGE('',*,*,#6528,.F.);
#8688=ORIENTED_EDGE('',*,*,#6525,.F.);
#8689=ORIENTED_EDGE('',*,*,#6535,.F.);
#8690=ORIENTED_EDGE('',*,*,#6561,.F.);
#8691=ORIENTED_EDGE('',*,*,#6372,.F.);
#8692=ORIENTED_EDGE('',*,*,#6558,.F.);
#8693=ORIENTED_EDGE('',*,*,#6559,.F.);
#8694=ORIENTED_EDGE('',*,*,#6328,.F.);
#8695=ORIENTED_EDGE('',*,*,#6560,.F.);
#8696=ORIENTED_EDGE('',*,*,#6536,.F.);
#8697=ORIENTED_EDGE('',*,*,#6527,.F.);
#8698=ORIENTED_EDGE('',*,*,#6533,.F.);
#8699=ORIENTED_EDGE('',*,*,#6562,.T.);
#8700=ORIENTED_EDGE('',*,*,#6563,.T.);
#8701=ORIENTED_EDGE('',*,*,#6564,.T.);
#8702=ORIENTED_EDGE('',*,*,#6565,.T.);
#8703=ORIENTED_EDGE('',*,*,#6562,.F.);
#8704=ORIENTED_EDGE('',*,*,#6566,.T.);
#8705=ORIENTED_EDGE('',*,*,#6567,.F.);
#8706=ORIENTED_EDGE('',*,*,#6568,.T.);
#8707=ORIENTED_EDGE('',*,*,#6569,.F.);
#8708=ORIENTED_EDGE('',*,*,#6570,.T.);
#8709=ORIENTED_EDGE('',*,*,#6571,.F.);
#8710=ORIENTED_EDGE('',*,*,#6572,.F.);
#8711=ORIENTED_EDGE('',*,*,#6573,.T.);
#8712=ORIENTED_EDGE('',*,*,#6574,.T.);
#8713=ORIENTED_EDGE('',*,*,#6575,.T.);
#8714=ORIENTED_EDGE('',*,*,#6576,.F.);
#8715=ORIENTED_EDGE('',*,*,#6577,.T.);
#8716=ORIENTED_EDGE('',*,*,#6578,.T.);
#8717=ORIENTED_EDGE('',*,*,#6579,.T.);
#8718=ORIENTED_EDGE('',*,*,#6565,.F.);
#8719=ORIENTED_EDGE('',*,*,#6580,.F.);
#8720=ORIENTED_EDGE('',*,*,#6581,.F.);
#8721=ORIENTED_EDGE('',*,*,#6566,.F.);
#8722=ORIENTED_EDGE('',*,*,#6582,.T.);
#8723=ORIENTED_EDGE('',*,*,#6583,.T.);
#8724=ORIENTED_EDGE('',*,*,#6584,.T.);
#8725=ORIENTED_EDGE('',*,*,#6585,.T.);
#8726=ORIENTED_EDGE('',*,*,#6582,.F.);
#8727=ORIENTED_EDGE('',*,*,#6586,.T.);
#8728=ORIENTED_EDGE('',*,*,#6587,.F.);
#8729=ORIENTED_EDGE('',*,*,#6588,.T.);
#8730=ORIENTED_EDGE('',*,*,#6589,.F.);
#8731=ORIENTED_EDGE('',*,*,#6590,.F.);
#8732=ORIENTED_EDGE('',*,*,#6591,.F.);
#8733=ORIENTED_EDGE('',*,*,#6592,.F.);
#8734=ORIENTED_EDGE('',*,*,#6593,.T.);
#8735=ORIENTED_EDGE('',*,*,#6594,.F.);
#8736=ORIENTED_EDGE('',*,*,#6595,.T.);
#8737=ORIENTED_EDGE('',*,*,#6596,.T.);
#8738=ORIENTED_EDGE('',*,*,#6597,.T.);
#8739=ORIENTED_EDGE('',*,*,#6598,.F.);
#8740=ORIENTED_EDGE('',*,*,#6599,.T.);
#8741=ORIENTED_EDGE('',*,*,#6600,.T.);
#8742=ORIENTED_EDGE('',*,*,#6601,.T.);
#8743=ORIENTED_EDGE('',*,*,#6602,.T.);
#8744=ORIENTED_EDGE('',*,*,#6585,.F.);
#8745=ORIENTED_EDGE('',*,*,#6603,.F.);
#8746=ORIENTED_EDGE('',*,*,#6604,.F.);
#8747=ORIENTED_EDGE('',*,*,#6586,.F.);
#8748=ORIENTED_EDGE('',*,*,#6605,.T.);
#8749=ORIENTED_EDGE('',*,*,#6606,.T.);
#8750=ORIENTED_EDGE('',*,*,#6567,.T.);
#8751=ORIENTED_EDGE('',*,*,#6581,.T.);
#8752=ORIENTED_EDGE('',*,*,#6606,.F.);
#8753=ORIENTED_EDGE('',*,*,#6607,.F.);
#8754=ORIENTED_EDGE('',*,*,#6608,.F.);
#8755=ORIENTED_EDGE('',*,*,#6568,.F.);
#8756=ORIENTED_EDGE('',*,*,#6609,.T.);
#8757=ORIENTED_EDGE('',*,*,#6610,.T.);
#8758=ORIENTED_EDGE('',*,*,#6587,.T.);
#8759=ORIENTED_EDGE('',*,*,#6604,.T.);
#8760=ORIENTED_EDGE('',*,*,#6610,.F.);
#8761=ORIENTED_EDGE('',*,*,#6611,.F.);
#8762=ORIENTED_EDGE('',*,*,#6612,.F.);
#8763=ORIENTED_EDGE('',*,*,#6588,.F.);
#8764=ORIENTED_EDGE('',*,*,#6612,.T.);
#8765=ORIENTED_EDGE('',*,*,#6613,.F.);
#8766=ORIENTED_EDGE('',*,*,#6614,.T.);
#8767=ORIENTED_EDGE('',*,*,#6615,.T.);
#8768=ORIENTED_EDGE('',*,*,#6589,.T.);
#8769=ORIENTED_EDGE('',*,*,#6584,.F.);
#8770=ORIENTED_EDGE('',*,*,#6616,.T.);
#8771=ORIENTED_EDGE('',*,*,#6617,.T.);
#8772=ORIENTED_EDGE('',*,*,#6618,.T.);
#8773=ORIENTED_EDGE('',*,*,#6619,.T.);
#8774=ORIENTED_EDGE('',*,*,#6620,.T.);
#8775=ORIENTED_EDGE('',*,*,#6621,.T.);
#8776=ORIENTED_EDGE('',*,*,#6622,.T.);
#8777=ORIENTED_EDGE('',*,*,#6623,.T.);
#8778=ORIENTED_EDGE('',*,*,#6613,.T.);
#8779=ORIENTED_EDGE('',*,*,#6611,.T.);
#8780=ORIENTED_EDGE('',*,*,#6609,.F.);
#8781=ORIENTED_EDGE('',*,*,#6603,.T.);
#8782=ORIENTED_EDGE('',*,*,#6624,.F.);
#8783=ORIENTED_EDGE('',*,*,#6625,.F.);
#8784=ORIENTED_EDGE('',*,*,#6608,.T.);
#8785=ORIENTED_EDGE('',*,*,#6626,.T.);
#8786=ORIENTED_EDGE('',*,*,#6627,.T.);
#8787=ORIENTED_EDGE('',*,*,#6628,.T.);
#8788=ORIENTED_EDGE('',*,*,#6569,.T.);
#8789=ORIENTED_EDGE('',*,*,#6629,.F.);
#8790=ORIENTED_EDGE('',*,*,#6630,.T.);
#8791=ORIENTED_EDGE('',*,*,#6631,.F.);
#8792=ORIENTED_EDGE('',*,*,#6630,.F.);
#8793=ORIENTED_EDGE('',*,*,#6632,.F.);
#8794=ORIENTED_EDGE('',*,*,#6633,.F.);
#8795=ORIENTED_EDGE('',*,*,#6634,.T.);
#8796=ORIENTED_EDGE('',*,*,#6635,.F.);
#8797=ORIENTED_EDGE('',*,*,#6634,.F.);
#8798=ORIENTED_EDGE('',*,*,#6636,.F.);
#8799=ORIENTED_EDGE('',*,*,#6614,.F.);
#8800=ORIENTED_EDGE('',*,*,#6623,.F.);
#8801=ORIENTED_EDGE('',*,*,#6637,.F.);
#8802=ORIENTED_EDGE('',*,*,#6638,.F.);
#8803=ORIENTED_EDGE('',*,*,#6570,.F.);
#8804=ORIENTED_EDGE('',*,*,#6628,.F.);
#8805=ORIENTED_EDGE('',*,*,#6639,.F.);
#8806=ORIENTED_EDGE('',*,*,#6640,.F.);
#8807=ORIENTED_EDGE('',*,*,#6641,.F.);
#8808=ORIENTED_EDGE('',*,*,#6624,.T.);
#8809=ORIENTED_EDGE('',*,*,#6642,.T.);
#8810=ORIENTED_EDGE('',*,*,#6600,.F.);
#8811=ORIENTED_EDGE('',*,*,#6642,.F.);
#8812=ORIENTED_EDGE('',*,*,#6625,.T.);
#8813=ORIENTED_EDGE('',*,*,#6643,.T.);
#8814=ORIENTED_EDGE('',*,*,#6602,.F.);
#8815=ORIENTED_EDGE('',*,*,#6643,.F.);
#8816=ORIENTED_EDGE('',*,*,#6644,.T.);
#8817=ORIENTED_EDGE('',*,*,#6645,.T.);
#8818=ORIENTED_EDGE('',*,*,#6601,.F.);
#8819=ORIENTED_EDGE('',*,*,#6645,.F.);
#8820=ORIENTED_EDGE('',*,*,#6632,.T.);
#8821=ORIENTED_EDGE('',*,*,#6633,.T.);
#8822=ORIENTED_EDGE('',*,*,#6646,.T.);
#8823=ORIENTED_EDGE('',*,*,#6639,.T.);
#8824=ORIENTED_EDGE('',*,*,#6627,.F.);
#8825=ORIENTED_EDGE('',*,*,#6647,.T.);
#8826=ORIENTED_EDGE('',*,*,#6648,.T.);
#8827=ORIENTED_EDGE('',*,*,#6640,.T.);
#8828=ORIENTED_EDGE('',*,*,#6646,.F.);
#8829=ORIENTED_EDGE('',*,*,#6649,.F.);
#8830=ORIENTED_EDGE('',*,*,#6650,.T.);
#8831=ORIENTED_EDGE('',*,*,#6579,.F.);
#8832=ORIENTED_EDGE('',*,*,#6650,.F.);
#8833=ORIENTED_EDGE('',*,*,#6651,.F.);
#8834=ORIENTED_EDGE('',*,*,#6652,.T.);
#8835=ORIENTED_EDGE('',*,*,#6578,.F.);
#8836=ORIENTED_EDGE('',*,*,#6652,.F.);
#8837=ORIENTED_EDGE('',*,*,#6653,.F.);
#8838=ORIENTED_EDGE('',*,*,#6654,.T.);
#8839=ORIENTED_EDGE('',*,*,#6655,.F.);
#8840=ORIENTED_EDGE('',*,*,#6654,.F.);
#8841=ORIENTED_EDGE('',*,*,#6590,.T.);
#8842=ORIENTED_EDGE('',*,*,#6615,.F.);
#8843=ORIENTED_EDGE('',*,*,#6636,.T.);
#8844=ORIENTED_EDGE('',*,*,#6656,.T.);
#8845=ORIENTED_EDGE('',*,*,#6629,.T.);
#8846=ORIENTED_EDGE('',*,*,#6656,.F.);
#8847=ORIENTED_EDGE('',*,*,#6638,.T.);
#8848=ORIENTED_EDGE('',*,*,#6657,.T.);
#8849=ORIENTED_EDGE('',*,*,#6658,.F.);
#8850=ORIENTED_EDGE('',*,*,#6659,.T.);
#8851=ORIENTED_EDGE('',*,*,#6660,.F.);
#8852=ORIENTED_EDGE('',*,*,#6661,.T.);
#8853=ORIENTED_EDGE('',*,*,#6575,.F.);
#8854=ORIENTED_EDGE('',*,*,#6662,.T.);
#8855=ORIENTED_EDGE('',*,*,#6663,.F.);
#8856=ORIENTED_EDGE('',*,*,#6664,.T.);
#8857=ORIENTED_EDGE('',*,*,#6618,.F.);
#8858=ORIENTED_EDGE('',*,*,#6665,.F.);
#8859=ORIENTED_EDGE('',*,*,#6597,.F.);
#8860=ORIENTED_EDGE('',*,*,#6666,.T.);
#8861=ORIENTED_EDGE('',*,*,#6667,.F.);
#8862=ORIENTED_EDGE('',*,*,#6668,.F.);
#8863=ORIENTED_EDGE('',*,*,#6669,.F.);
#8864=ORIENTED_EDGE('',*,*,#6670,.T.);
#8865=ORIENTED_EDGE('',*,*,#6573,.F.);
#8866=ORIENTED_EDGE('',*,*,#6671,.F.);
#8867=ORIENTED_EDGE('',*,*,#6672,.F.);
#8868=ORIENTED_EDGE('',*,*,#6673,.T.);
#8869=ORIENTED_EDGE('',*,*,#6593,.F.);
#8870=ORIENTED_EDGE('',*,*,#6674,.F.);
#8871=ORIENTED_EDGE('',*,*,#6620,.F.);
#8872=ORIENTED_EDGE('',*,*,#6675,.T.);
#8873=ORIENTED_EDGE('',*,*,#6621,.F.);
#8874=ORIENTED_EDGE('',*,*,#6674,.T.);
#8875=ORIENTED_EDGE('',*,*,#6592,.T.);
#8876=ORIENTED_EDGE('',*,*,#6676,.F.);
#8877=ORIENTED_EDGE('',*,*,#6677,.T.);
#8878=ORIENTED_EDGE('',*,*,#6678,.T.);
#8879=ORIENTED_EDGE('',*,*,#6576,.T.);
#8880=ORIENTED_EDGE('',*,*,#6668,.T.);
#8881=ORIENTED_EDGE('',*,*,#6648,.F.);
#8882=ORIENTED_EDGE('',*,*,#6679,.T.);
#8883=ORIENTED_EDGE('',*,*,#6680,.T.);
#8884=ORIENTED_EDGE('',*,*,#6571,.T.);
#8885=ORIENTED_EDGE('',*,*,#6641,.T.);
#8886=ORIENTED_EDGE('',*,*,#6617,.F.);
#8887=ORIENTED_EDGE('',*,*,#6681,.T.);
#8888=ORIENTED_EDGE('',*,*,#6598,.T.);
#8889=ORIENTED_EDGE('',*,*,#6665,.T.);
#8890=ORIENTED_EDGE('',*,*,#6663,.T.);
#8891=ORIENTED_EDGE('',*,*,#6682,.T.);
#8892=ORIENTED_EDGE('',*,*,#6669,.T.);
#8893=ORIENTED_EDGE('',*,*,#6683,.T.);
#8894=ORIENTED_EDGE('',*,*,#6684,.T.);
#8895=ORIENTED_EDGE('',*,*,#6671,.T.);
#8896=ORIENTED_EDGE('',*,*,#6572,.T.);
#8897=ORIENTED_EDGE('',*,*,#6680,.F.);
#8898=ORIENTED_EDGE('',*,*,#6676,.T.);
#8899=ORIENTED_EDGE('',*,*,#6591,.T.);
#8900=ORIENTED_EDGE('',*,*,#6657,.F.);
#8901=ORIENTED_EDGE('',*,*,#6637,.T.);
#8902=ORIENTED_EDGE('',*,*,#6622,.F.);
#8903=ORIENTED_EDGE('',*,*,#6564,.F.);
#8904=ORIENTED_EDGE('',*,*,#6685,.T.);
#8905=ORIENTED_EDGE('',*,*,#6677,.F.);
#8906=ORIENTED_EDGE('',*,*,#6667,.T.);
#8907=ORIENTED_EDGE('',*,*,#6686,.F.);
#8908=ORIENTED_EDGE('',*,*,#6687,.T.);
#8909=ORIENTED_EDGE('',*,*,#6688,.T.);
#8910=ORIENTED_EDGE('',*,*,#6672,.T.);
#8911=ORIENTED_EDGE('',*,*,#6684,.F.);
#8912=ORIENTED_EDGE('',*,*,#6679,.F.);
#8913=ORIENTED_EDGE('',*,*,#6647,.F.);
#8914=ORIENTED_EDGE('',*,*,#6626,.F.);
#8915=ORIENTED_EDGE('',*,*,#6607,.T.);
#8916=ORIENTED_EDGE('',*,*,#6605,.F.);
#8917=ORIENTED_EDGE('',*,*,#6580,.T.);
#8918=ORIENTED_EDGE('',*,*,#6651,.T.);
#8919=ORIENTED_EDGE('',*,*,#6653,.T.);
#8920=ORIENTED_EDGE('',*,*,#6649,.T.);
#8921=ORIENTED_EDGE('',*,*,#6631,.T.);
#8922=ORIENTED_EDGE('',*,*,#6644,.F.);
#8923=ORIENTED_EDGE('',*,*,#6635,.T.);
#8924=ORIENTED_EDGE('',*,*,#6655,.T.);
#8925=ORIENTED_EDGE('',*,*,#6563,.F.);
#8926=ORIENTED_EDGE('',*,*,#6577,.F.);
#8927=ORIENTED_EDGE('',*,*,#6678,.F.);
#8928=ORIENTED_EDGE('',*,*,#6685,.F.);
#8929=ORIENTED_EDGE('',*,*,#6583,.F.);
#8930=ORIENTED_EDGE('',*,*,#6599,.F.);
#8931=ORIENTED_EDGE('',*,*,#6681,.F.);
#8932=ORIENTED_EDGE('',*,*,#6616,.F.);
#8933=ORIENTED_EDGE('',*,*,#6688,.F.);
#8934=ORIENTED_EDGE('',*,*,#6689,.T.);
#8935=ORIENTED_EDGE('',*,*,#6658,.T.);
#8936=ORIENTED_EDGE('',*,*,#6690,.T.);
#8937=ORIENTED_EDGE('',*,*,#6594,.T.);
#8938=ORIENTED_EDGE('',*,*,#6673,.F.);
#8939=ORIENTED_EDGE('',*,*,#6596,.F.);
#8940=ORIENTED_EDGE('',*,*,#6691,.T.);
#8941=ORIENTED_EDGE('',*,*,#6660,.T.);
#8942=ORIENTED_EDGE('',*,*,#6692,.T.);
#8943=ORIENTED_EDGE('',*,*,#6686,.T.);
#8944=ORIENTED_EDGE('',*,*,#6666,.F.);
#8945=ORIENTED_EDGE('',*,*,#6662,.F.);
#8946=ORIENTED_EDGE('',*,*,#6574,.F.);
#8947=ORIENTED_EDGE('',*,*,#6670,.F.);
#8948=ORIENTED_EDGE('',*,*,#6682,.F.);
#8949=ORIENTED_EDGE('',*,*,#6664,.F.);
#8950=ORIENTED_EDGE('',*,*,#6683,.F.);
#8951=ORIENTED_EDGE('',*,*,#6675,.F.);
#8952=ORIENTED_EDGE('',*,*,#6619,.F.);
#8953=ORIENTED_EDGE('',*,*,#6692,.F.);
#8954=ORIENTED_EDGE('',*,*,#6659,.F.);
#8955=ORIENTED_EDGE('',*,*,#6689,.F.);
#8956=ORIENTED_EDGE('',*,*,#6687,.F.);
#8957=ORIENTED_EDGE('',*,*,#6691,.F.);
#8958=ORIENTED_EDGE('',*,*,#6595,.F.);
#8959=ORIENTED_EDGE('',*,*,#6690,.F.);
#8960=ORIENTED_EDGE('',*,*,#6661,.F.);
#8961=ORIENTED_EDGE('',*,*,#6693,.F.);
#8962=ORIENTED_EDGE('',*,*,#6694,.T.);
#8963=ORIENTED_EDGE('',*,*,#6695,.F.);
#8964=ORIENTED_EDGE('',*,*,#6694,.F.);
#8965=ORIENTED_EDGE('',*,*,#6696,.F.);
#8966=ORIENTED_EDGE('',*,*,#6697,.T.);
#8967=ORIENTED_EDGE('',*,*,#6698,.F.);
#8968=ORIENTED_EDGE('',*,*,#6697,.F.);
#8969=ORIENTED_EDGE('',*,*,#6699,.F.);
#8970=ORIENTED_EDGE('',*,*,#6700,.F.);
#8971=ORIENTED_EDGE('',*,*,#6701,.T.);
#8972=ORIENTED_EDGE('',*,*,#6702,.F.);
#8973=ORIENTED_EDGE('',*,*,#6701,.F.);
#8974=ORIENTED_EDGE('',*,*,#6703,.T.);
#8975=ORIENTED_EDGE('',*,*,#6704,.T.);
#8976=ORIENTED_EDGE('',*,*,#6693,.T.);
#8977=ORIENTED_EDGE('',*,*,#6704,.F.);
#8978=ORIENTED_EDGE('',*,*,#6699,.T.);
#8979=ORIENTED_EDGE('',*,*,#6700,.T.);
#8980=ORIENTED_EDGE('',*,*,#6705,.T.);
#8981=ORIENTED_EDGE('',*,*,#6696,.T.);
#8982=ORIENTED_EDGE('',*,*,#6705,.F.);
#8983=ORIENTED_EDGE('',*,*,#6698,.T.);
#8984=ORIENTED_EDGE('',*,*,#6702,.T.);
#8985=ORIENTED_EDGE('',*,*,#6703,.F.);
#8986=ORIENTED_EDGE('',*,*,#6695,.T.);
#8987=ORIENTED_EDGE('',*,*,#6706,.T.);
#8988=ORIENTED_EDGE('',*,*,#6707,.T.);
#8989=ORIENTED_EDGE('',*,*,#6708,.T.);
#8990=ORIENTED_EDGE('',*,*,#6707,.F.);
#8991=ORIENTED_EDGE('',*,*,#6709,.T.);
#8992=ORIENTED_EDGE('',*,*,#6710,.T.);
#8993=ORIENTED_EDGE('',*,*,#6711,.T.);
#8994=ORIENTED_EDGE('',*,*,#6710,.F.);
#8995=ORIENTED_EDGE('',*,*,#6712,.T.);
#8996=ORIENTED_EDGE('',*,*,#6713,.T.);
#8997=ORIENTED_EDGE('',*,*,#6714,.T.);
#8998=ORIENTED_EDGE('',*,*,#6713,.F.);
#8999=ORIENTED_EDGE('',*,*,#6715,.T.);
#9000=ORIENTED_EDGE('',*,*,#6716,.F.);
#9001=ORIENTED_EDGE('',*,*,#6717,.T.);
#9002=ORIENTED_EDGE('',*,*,#6706,.F.);
#9003=ORIENTED_EDGE('',*,*,#6717,.F.);
#9004=ORIENTED_EDGE('',*,*,#6712,.F.);
#9005=ORIENTED_EDGE('',*,*,#6718,.T.);
#9006=ORIENTED_EDGE('',*,*,#6709,.F.);
#9007=ORIENTED_EDGE('',*,*,#6718,.F.);
#9008=ORIENTED_EDGE('',*,*,#6715,.F.);
#9009=ORIENTED_EDGE('',*,*,#6711,.F.);
#9010=ORIENTED_EDGE('',*,*,#6714,.F.);
#9011=ORIENTED_EDGE('',*,*,#6716,.T.);
#9012=ORIENTED_EDGE('',*,*,#6708,.F.);
#9013=ORIENTED_EDGE('',*,*,#6719,.F.);
#9014=ORIENTED_EDGE('',*,*,#6720,.F.);
#9015=ORIENTED_EDGE('',*,*,#6721,.T.);
#9016=ORIENTED_EDGE('',*,*,#6722,.F.);
#9017=ORIENTED_EDGE('',*,*,#6721,.F.);
#9018=ORIENTED_EDGE('',*,*,#6723,.F.);
#9019=ORIENTED_EDGE('',*,*,#6724,.F.);
#9020=ORIENTED_EDGE('',*,*,#6725,.F.);
#9021=ORIENTED_EDGE('',*,*,#6726,.F.);
#9022=ORIENTED_EDGE('',*,*,#6727,.T.);
#9023=ORIENTED_EDGE('',*,*,#6728,.T.);
#9024=ORIENTED_EDGE('',*,*,#6729,.T.);
#9025=ORIENTED_EDGE('',*,*,#6730,.T.);
#9026=ORIENTED_EDGE('',*,*,#6731,.T.);
#9027=ORIENTED_EDGE('',*,*,#6732,.T.);
#9028=ORIENTED_EDGE('',*,*,#6733,.T.);
#9029=ORIENTED_EDGE('',*,*,#6734,.T.);
#9030=ORIENTED_EDGE('',*,*,#6735,.T.);
#9031=ORIENTED_EDGE('',*,*,#6736,.T.);
#9032=ORIENTED_EDGE('',*,*,#6737,.T.);
#9033=ORIENTED_EDGE('',*,*,#6738,.T.);
#9034=ORIENTED_EDGE('',*,*,#6739,.T.);
#9035=ORIENTED_EDGE('',*,*,#6740,.T.);
#9036=ORIENTED_EDGE('',*,*,#6741,.T.);
#9037=ORIENTED_EDGE('',*,*,#6742,.T.);
#9038=ORIENTED_EDGE('',*,*,#6743,.T.);
#9039=ORIENTED_EDGE('',*,*,#6744,.T.);
#9040=ORIENTED_EDGE('',*,*,#6745,.T.);
#9041=ORIENTED_EDGE('',*,*,#6746,.T.);
#9042=ORIENTED_EDGE('',*,*,#6725,.T.);
#9043=ORIENTED_EDGE('',*,*,#6747,.T.);
#9044=ORIENTED_EDGE('',*,*,#6748,.T.);
#9045=ORIENTED_EDGE('',*,*,#6749,.T.);
#9046=ORIENTED_EDGE('',*,*,#6750,.T.);
#9047=ORIENTED_EDGE('',*,*,#6751,.T.);
#9048=ORIENTED_EDGE('',*,*,#6752,.T.);
#9049=ORIENTED_EDGE('',*,*,#6753,.T.);
#9050=ORIENTED_EDGE('',*,*,#6754,.T.);
#9051=ORIENTED_EDGE('',*,*,#6755,.T.);
#9052=ORIENTED_EDGE('',*,*,#6756,.T.);
#9053=ORIENTED_EDGE('',*,*,#6757,.T.);
#9054=ORIENTED_EDGE('',*,*,#6758,.F.);
#9055=ORIENTED_EDGE('',*,*,#6719,.T.);
#9056=ORIENTED_EDGE('',*,*,#6720,.T.);
#9057=ORIENTED_EDGE('',*,*,#6759,.T.);
#9058=ORIENTED_EDGE('',*,*,#6758,.T.);
#9059=ORIENTED_EDGE('',*,*,#6759,.F.);
#9060=ORIENTED_EDGE('',*,*,#6760,.T.);
#9061=ORIENTED_EDGE('',*,*,#6761,.T.);
#9062=ORIENTED_EDGE('',*,*,#6762,.T.);
#9063=ORIENTED_EDGE('',*,*,#6756,.F.);
#9064=ORIENTED_EDGE('',*,*,#6763,.T.);
#9065=ORIENTED_EDGE('',*,*,#6764,.T.);
#9066=ORIENTED_EDGE('',*,*,#6765,.T.);
#9067=ORIENTED_EDGE('',*,*,#6745,.F.);
#9068=ORIENTED_EDGE('',*,*,#6766,.T.);
#9069=ORIENTED_EDGE('',*,*,#6767,.T.);
#9070=ORIENTED_EDGE('',*,*,#6768,.T.);
#9071=ORIENTED_EDGE('',*,*,#6752,.F.);
#9072=ORIENTED_EDGE('',*,*,#6722,.T.);
#9073=ORIENTED_EDGE('',*,*,#6769,.T.);
#9074=ORIENTED_EDGE('',*,*,#6770,.T.);
#9075=ORIENTED_EDGE('',*,*,#6771,.T.);
#9076=ORIENTED_EDGE('',*,*,#6748,.F.);
#9077=ORIENTED_EDGE('',*,*,#6772,.T.);
#9078=ORIENTED_EDGE('',*,*,#6773,.T.);
#9079=ORIENTED_EDGE('',*,*,#6774,.F.);
#9080=ORIENTED_EDGE('',*,*,#6735,.F.);
#9081=ORIENTED_EDGE('',*,*,#6771,.F.);
#9082=ORIENTED_EDGE('',*,*,#6775,.T.);
#9083=ORIENTED_EDGE('',*,*,#6736,.F.);
#9084=ORIENTED_EDGE('',*,*,#6774,.T.);
#9085=ORIENTED_EDGE('',*,*,#6776,.T.);
#9086=ORIENTED_EDGE('',*,*,#6749,.F.);
#9087=ORIENTED_EDGE('',*,*,#6734,.F.);
#9088=ORIENTED_EDGE('',*,*,#6777,.T.);
#9089=ORIENTED_EDGE('',*,*,#6766,.F.);
#9090=ORIENTED_EDGE('',*,*,#6751,.F.);
#9091=ORIENTED_EDGE('',*,*,#6778,.T.);
#9092=ORIENTED_EDGE('',*,*,#6772,.F.);
#9093=ORIENTED_EDGE('',*,*,#6762,.F.);
#9094=ORIENTED_EDGE('',*,*,#6779,.T.);
#9095=ORIENTED_EDGE('',*,*,#6728,.F.);
#9096=ORIENTED_EDGE('',*,*,#6780,.F.);
#9097=ORIENTED_EDGE('',*,*,#6781,.T.);
#9098=ORIENTED_EDGE('',*,*,#6757,.F.);
#9099=ORIENTED_EDGE('',*,*,#6742,.F.);
#9100=ORIENTED_EDGE('',*,*,#6782,.T.);
#9101=ORIENTED_EDGE('',*,*,#6763,.F.);
#9102=ORIENTED_EDGE('',*,*,#6744,.F.);
#9103=ORIENTED_EDGE('',*,*,#6783,.T.);
#9104=ORIENTED_EDGE('',*,*,#6784,.T.);
#9105=ORIENTED_EDGE('',*,*,#6784,.F.);
#9106=ORIENTED_EDGE('',*,*,#6785,.T.);
#9107=ORIENTED_EDGE('',*,*,#6780,.T.);
#9108=ORIENTED_EDGE('',*,*,#6727,.F.);
#9109=ORIENTED_EDGE('',*,*,#6786,.F.);
#9110=ORIENTED_EDGE('',*,*,#6723,.T.);
#9111=ORIENTED_EDGE('',*,*,#6787,.T.);
#9112=ORIENTED_EDGE('',*,*,#6739,.F.);
#9113=ORIENTED_EDGE('',*,*,#6738,.F.);
#9114=ORIENTED_EDGE('',*,*,#6788,.T.);
#9115=ORIENTED_EDGE('',*,*,#6769,.F.);
#9116=ORIENTED_EDGE('',*,*,#6747,.F.);
#9117=ORIENTED_EDGE('',*,*,#6724,.T.);
#9118=ORIENTED_EDGE('',*,*,#6786,.T.);
#9119=ORIENTED_EDGE('',*,*,#6765,.F.);
#9120=ORIENTED_EDGE('',*,*,#6789,.T.);
#9121=ORIENTED_EDGE('',*,*,#6740,.F.);
#9122=ORIENTED_EDGE('',*,*,#6787,.F.);
#9123=ORIENTED_EDGE('',*,*,#6726,.T.);
#9124=ORIENTED_EDGE('',*,*,#6746,.F.);
#9125=ORIENTED_EDGE('',*,*,#6730,.F.);
#9126=ORIENTED_EDGE('',*,*,#6790,.T.);
#9127=ORIENTED_EDGE('',*,*,#6760,.F.);
#9128=ORIENTED_EDGE('',*,*,#6755,.F.);
#9129=ORIENTED_EDGE('',*,*,#6791,.T.);
#9130=ORIENTED_EDGE('',*,*,#6792,.F.);
#9131=ORIENTED_EDGE('',*,*,#6768,.F.);
#9132=ORIENTED_EDGE('',*,*,#6793,.T.);
#9133=ORIENTED_EDGE('',*,*,#6732,.F.);
#9134=ORIENTED_EDGE('',*,*,#6794,.T.);
#9135=ORIENTED_EDGE('',*,*,#6795,.T.);
#9136=ORIENTED_EDGE('',*,*,#6753,.F.);
#9137=ORIENTED_EDGE('',*,*,#6792,.T.);
#9138=ORIENTED_EDGE('',*,*,#6796,.T.);
#9139=ORIENTED_EDGE('',*,*,#6794,.F.);
#9140=ORIENTED_EDGE('',*,*,#6731,.F.);
#9141=ORIENTED_EDGE('',*,*,#6733,.F.);
#9142=ORIENTED_EDGE('',*,*,#6793,.F.);
#9143=ORIENTED_EDGE('',*,*,#6767,.F.);
#9144=ORIENTED_EDGE('',*,*,#6777,.F.);
#9145=ORIENTED_EDGE('',*,*,#6761,.F.);
#9146=ORIENTED_EDGE('',*,*,#6790,.F.);
#9147=ORIENTED_EDGE('',*,*,#6729,.F.);
#9148=ORIENTED_EDGE('',*,*,#6779,.F.);
#9149=ORIENTED_EDGE('',*,*,#6741,.F.);
#9150=ORIENTED_EDGE('',*,*,#6789,.F.);
#9151=ORIENTED_EDGE('',*,*,#6764,.F.);
#9152=ORIENTED_EDGE('',*,*,#6782,.F.);
#9153=ORIENTED_EDGE('',*,*,#6770,.F.);
#9154=ORIENTED_EDGE('',*,*,#6788,.F.);
#9155=ORIENTED_EDGE('',*,*,#6737,.F.);
#9156=ORIENTED_EDGE('',*,*,#6775,.F.);
#9157=ORIENTED_EDGE('',*,*,#6776,.F.);
#9158=ORIENTED_EDGE('',*,*,#6773,.F.);
#9159=ORIENTED_EDGE('',*,*,#6778,.F.);
#9160=ORIENTED_EDGE('',*,*,#6750,.F.);
#9161=ORIENTED_EDGE('',*,*,#6795,.F.);
#9162=ORIENTED_EDGE('',*,*,#6796,.F.);
#9163=ORIENTED_EDGE('',*,*,#6791,.F.);
#9164=ORIENTED_EDGE('',*,*,#6754,.F.);
#9165=ORIENTED_EDGE('',*,*,#6781,.F.);
#9166=ORIENTED_EDGE('',*,*,#6785,.F.);
#9167=ORIENTED_EDGE('',*,*,#6783,.F.);
#9168=ORIENTED_EDGE('',*,*,#6743,.F.);
#9169=ORIENTED_EDGE('',*,*,#6797,.F.);
#9170=ORIENTED_EDGE('',*,*,#6798,.T.);
#9171=ORIENTED_EDGE('',*,*,#6799,.F.);
#9172=ORIENTED_EDGE('',*,*,#6798,.F.);
#9173=ORIENTED_EDGE('',*,*,#6800,.F.);
#9174=ORIENTED_EDGE('',*,*,#6801,.T.);
#9175=ORIENTED_EDGE('',*,*,#6802,.F.);
#9176=ORIENTED_EDGE('',*,*,#6803,.F.);
#9177=ORIENTED_EDGE('',*,*,#6801,.F.);
#9178=ORIENTED_EDGE('',*,*,#6804,.F.);
#9179=ORIENTED_EDGE('',*,*,#6805,.T.);
#9180=ORIENTED_EDGE('',*,*,#6806,.F.);
#9181=ORIENTED_EDGE('',*,*,#6807,.F.);
#9182=ORIENTED_EDGE('',*,*,#6805,.F.);
#9183=ORIENTED_EDGE('',*,*,#6802,.T.);
#9184=ORIENTED_EDGE('',*,*,#6803,.T.);
#9185=ORIENTED_EDGE('',*,*,#6808,.T.);
#9186=ORIENTED_EDGE('',*,*,#6806,.T.);
#9187=ORIENTED_EDGE('',*,*,#6807,.T.);
#9188=ORIENTED_EDGE('',*,*,#6808,.F.);
#9189=ORIENTED_EDGE('',*,*,#6809,.T.);
#9190=ORIENTED_EDGE('',*,*,#6810,.T.);
#9191=ORIENTED_EDGE('',*,*,#6811,.F.);
#9192=ORIENTED_EDGE('',*,*,#6810,.F.);
#9193=ORIENTED_EDGE('',*,*,#6812,.T.);
#9194=ORIENTED_EDGE('',*,*,#6813,.T.);
#9195=ORIENTED_EDGE('',*,*,#6814,.T.);
#9196=ORIENTED_EDGE('',*,*,#6815,.T.);
#9197=ORIENTED_EDGE('',*,*,#6816,.F.);
#9198=ORIENTED_EDGE('',*,*,#6815,.F.);
#9199=ORIENTED_EDGE('',*,*,#6817,.T.);
#9200=ORIENTED_EDGE('',*,*,#6818,.T.);
#9201=ORIENTED_EDGE('',*,*,#6819,.T.);
#9202=ORIENTED_EDGE('',*,*,#6820,.T.);
#9203=ORIENTED_EDGE('',*,*,#6821,.F.);
#9204=ORIENTED_EDGE('',*,*,#6820,.F.);
#9205=ORIENTED_EDGE('',*,*,#6822,.F.);
#9206=ORIENTED_EDGE('',*,*,#6823,.T.);
#9207=ORIENTED_EDGE('',*,*,#6797,.T.);
#9208=ORIENTED_EDGE('',*,*,#6823,.F.);
#9209=ORIENTED_EDGE('',*,*,#6824,.T.);
#9210=ORIENTED_EDGE('',*,*,#6825,.T.);
#9211=ORIENTED_EDGE('',*,*,#6826,.F.);
#9212=ORIENTED_EDGE('',*,*,#6825,.F.);
#9213=ORIENTED_EDGE('',*,*,#6827,.T.);
#9214=ORIENTED_EDGE('',*,*,#6828,.T.);
#9215=ORIENTED_EDGE('',*,*,#6829,.F.);
#9216=ORIENTED_EDGE('',*,*,#6828,.F.);
#9217=ORIENTED_EDGE('',*,*,#6830,.T.);
#9218=ORIENTED_EDGE('',*,*,#6831,.T.);
#9219=ORIENTED_EDGE('',*,*,#6832,.T.);
#9220=ORIENTED_EDGE('',*,*,#6833,.F.);
#9221=ORIENTED_EDGE('',*,*,#6834,.F.);
#9222=ORIENTED_EDGE('',*,*,#6835,.T.);
#9223=ORIENTED_EDGE('',*,*,#6836,.F.);
#9224=ORIENTED_EDGE('',*,*,#6835,.F.);
#9225=ORIENTED_EDGE('',*,*,#6837,.F.);
#9226=ORIENTED_EDGE('',*,*,#6838,.T.);
#9227=ORIENTED_EDGE('',*,*,#6839,.T.);
#9228=ORIENTED_EDGE('',*,*,#6840,.F.);
#9229=ORIENTED_EDGE('',*,*,#6812,.F.);
#9230=ORIENTED_EDGE('',*,*,#6841,.T.);
#9231=ORIENTED_EDGE('',*,*,#6842,.T.);
#9232=ORIENTED_EDGE('',*,*,#6843,.F.);
#9233=ORIENTED_EDGE('',*,*,#6844,.F.);
#9234=ORIENTED_EDGE('',*,*,#6845,.T.);
#9235=ORIENTED_EDGE('',*,*,#6813,.F.);
#9236=ORIENTED_EDGE('',*,*,#6845,.F.);
#9237=ORIENTED_EDGE('',*,*,#6846,.F.);
#9238=ORIENTED_EDGE('',*,*,#6847,.T.);
#9239=ORIENTED_EDGE('',*,*,#6814,.F.);
#9240=ORIENTED_EDGE('',*,*,#6847,.F.);
#9241=ORIENTED_EDGE('',*,*,#6848,.F.);
#9242=ORIENTED_EDGE('',*,*,#6849,.T.);
#9243=ORIENTED_EDGE('',*,*,#6850,.T.);
#9244=ORIENTED_EDGE('',*,*,#6851,.F.);
#9245=ORIENTED_EDGE('',*,*,#6817,.F.);
#9246=ORIENTED_EDGE('',*,*,#6852,.T.);
#9247=ORIENTED_EDGE('',*,*,#6853,.T.);
#9248=ORIENTED_EDGE('',*,*,#6854,.T.);
#9249=ORIENTED_EDGE('',*,*,#6831,.F.);
#9250=ORIENTED_EDGE('',*,*,#6855,.T.);
#9251=ORIENTED_EDGE('',*,*,#6856,.T.);
#9252=ORIENTED_EDGE('',*,*,#6857,.T.);
#9253=ORIENTED_EDGE('',*,*,#6833,.T.);
#9254=ORIENTED_EDGE('',*,*,#6858,.T.);
#9255=ORIENTED_EDGE('',*,*,#6859,.T.);
#9256=ORIENTED_EDGE('',*,*,#6860,.T.);
#9257=ORIENTED_EDGE('',*,*,#6861,.T.);
#9258=ORIENTED_EDGE('',*,*,#6862,.T.);
#9259=ORIENTED_EDGE('',*,*,#6863,.T.);
#9260=ORIENTED_EDGE('',*,*,#6864,.T.);
#9261=ORIENTED_EDGE('',*,*,#6837,.T.);
#9262=ORIENTED_EDGE('',*,*,#6824,.F.);
#9263=ORIENTED_EDGE('',*,*,#6827,.F.);
#9264=ORIENTED_EDGE('',*,*,#6865,.F.);
#9265=ORIENTED_EDGE('',*,*,#6866,.T.);
#9266=ORIENTED_EDGE('',*,*,#6855,.F.);
#9267=ORIENTED_EDGE('',*,*,#6832,.F.);
#9268=ORIENTED_EDGE('',*,*,#6854,.F.);
#9269=ORIENTED_EDGE('',*,*,#6867,.T.);
#9270=ORIENTED_EDGE('',*,*,#6868,.F.);
#9271=ORIENTED_EDGE('',*,*,#6869,.T.);
#9272=ORIENTED_EDGE('',*,*,#6836,.T.);
#9273=ORIENTED_EDGE('',*,*,#6826,.T.);
#9274=ORIENTED_EDGE('',*,*,#6870,.T.);
#9275=ORIENTED_EDGE('',*,*,#6871,.T.);
#9276=ORIENTED_EDGE('',*,*,#6872,.F.);
#9277=ORIENTED_EDGE('',*,*,#6873,.T.);
#9278=ORIENTED_EDGE('',*,*,#6799,.T.);
#9279=ORIENTED_EDGE('',*,*,#6874,.T.);
#9280=ORIENTED_EDGE('',*,*,#6875,.T.);
#9281=ORIENTED_EDGE('',*,*,#6862,.F.);
#9282=ORIENTED_EDGE('',*,*,#6876,.T.);
#9283=ORIENTED_EDGE('',*,*,#6872,.T.);
#9284=ORIENTED_EDGE('',*,*,#6877,.T.);
#9285=ORIENTED_EDGE('',*,*,#6868,.T.);
#9286=ORIENTED_EDGE('',*,*,#6878,.T.);
#9287=ORIENTED_EDGE('',*,*,#6879,.T.);
#9288=ORIENTED_EDGE('',*,*,#6880,.T.);
#9289=ORIENTED_EDGE('',*,*,#6881,.T.);
#9290=ORIENTED_EDGE('',*,*,#6882,.T.);
#9291=ORIENTED_EDGE('',*,*,#6883,.T.);
#9292=ORIENTED_EDGE('',*,*,#6848,.T.);
#9293=ORIENTED_EDGE('',*,*,#6846,.T.);
#9294=ORIENTED_EDGE('',*,*,#6844,.T.);
#9295=ORIENTED_EDGE('',*,*,#6864,.F.);
#9296=ORIENTED_EDGE('',*,*,#6884,.T.);
#9297=ORIENTED_EDGE('',*,*,#6885,.T.);
#9298=ORIENTED_EDGE('',*,*,#6838,.F.);
#9299=ORIENTED_EDGE('',*,*,#6886,.T.);
#9300=ORIENTED_EDGE('',*,*,#6887,.T.);
#9301=ORIENTED_EDGE('',*,*,#6858,.F.);
#9302=ORIENTED_EDGE('',*,*,#6840,.T.);
#9303=ORIENTED_EDGE('',*,*,#6888,.F.);
#9304=ORIENTED_EDGE('',*,*,#6889,.T.);
#9305=ORIENTED_EDGE('',*,*,#6865,.T.);
#9306=ORIENTED_EDGE('',*,*,#6890,.T.);
#9307=ORIENTED_EDGE('',*,*,#6870,.F.);
#9308=ORIENTED_EDGE('',*,*,#6891,.T.);
#9309=ORIENTED_EDGE('',*,*,#6860,.F.);
#9310=ORIENTED_EDGE('',*,*,#6892,.T.);
#9311=ORIENTED_EDGE('',*,*,#6893,.F.);
#9312=ORIENTED_EDGE('',*,*,#6894,.F.);
#9313=ORIENTED_EDGE('',*,*,#6895,.F.);
#9314=ORIENTED_EDGE('',*,*,#6896,.F.);
#9315=ORIENTED_EDGE('',*,*,#6897,.F.);
#9316=ORIENTED_EDGE('',*,*,#6842,.F.);
#9317=ORIENTED_EDGE('',*,*,#6898,.F.);
#9318=ORIENTED_EDGE('',*,*,#6850,.F.);
#9319=ORIENTED_EDGE('',*,*,#6890,.F.);
#9320=ORIENTED_EDGE('',*,*,#6869,.F.);
#9321=ORIENTED_EDGE('',*,*,#6877,.F.);
#9322=ORIENTED_EDGE('',*,*,#6871,.F.);
#9323=ORIENTED_EDGE('',*,*,#6891,.F.);
#9324=ORIENTED_EDGE('',*,*,#6873,.F.);
#9325=ORIENTED_EDGE('',*,*,#6876,.F.);
#9326=ORIENTED_EDGE('',*,*,#6861,.F.);
#9327=ORIENTED_EDGE('',*,*,#6899,.T.);
#9328=ORIENTED_EDGE('',*,*,#6894,.T.);
#9329=ORIENTED_EDGE('',*,*,#6900,.F.);
#9330=ORIENTED_EDGE('',*,*,#6880,.F.);
#9331=ORIENTED_EDGE('',*,*,#6819,.F.);
#9332=ORIENTED_EDGE('',*,*,#6857,.F.);
#9333=ORIENTED_EDGE('',*,*,#6901,.T.);
#9334=ORIENTED_EDGE('',*,*,#6888,.T.);
#9335=ORIENTED_EDGE('',*,*,#6899,.F.);
#9336=ORIENTED_EDGE('',*,*,#6879,.F.);
#9337=ORIENTED_EDGE('',*,*,#6902,.T.);
#9338=ORIENTED_EDGE('',*,*,#6852,.F.);
#9339=ORIENTED_EDGE('',*,*,#6830,.F.);
#9340=ORIENTED_EDGE('',*,*,#6800,.T.);
#9341=ORIENTED_EDGE('',*,*,#6834,.T.);
#9342=ORIENTED_EDGE('',*,*,#6893,.T.);
#9343=ORIENTED_EDGE('',*,*,#6903,.T.);
#9344=ORIENTED_EDGE('',*,*,#6886,.F.);
#9345=ORIENTED_EDGE('',*,*,#6839,.F.);
#9346=ORIENTED_EDGE('',*,*,#6885,.F.);
#9347=ORIENTED_EDGE('',*,*,#6904,.T.);
#9348=ORIENTED_EDGE('',*,*,#6874,.F.);
#9349=ORIENTED_EDGE('',*,*,#6900,.T.);
#9350=ORIENTED_EDGE('',*,*,#6804,.T.);
#9351=ORIENTED_EDGE('',*,*,#6829,.T.);
#9352=ORIENTED_EDGE('',*,*,#6905,.T.);
#9353=ORIENTED_EDGE('',*,*,#6896,.T.);
#9354=ORIENTED_EDGE('',*,*,#6906,.F.);
#9355=ORIENTED_EDGE('',*,*,#6882,.F.);
#9356=ORIENTED_EDGE('',*,*,#6821,.T.);
#9357=ORIENTED_EDGE('',*,*,#6843,.T.);
#9358=ORIENTED_EDGE('',*,*,#6897,.T.);
#9359=ORIENTED_EDGE('',*,*,#6905,.F.);
#9360=ORIENTED_EDGE('',*,*,#6881,.F.);
#9361=ORIENTED_EDGE('',*,*,#6818,.F.);
#9362=ORIENTED_EDGE('',*,*,#6851,.T.);
#9363=ORIENTED_EDGE('',*,*,#6898,.T.);
#9364=ORIENTED_EDGE('',*,*,#6841,.F.);
#9365=ORIENTED_EDGE('',*,*,#6906,.T.);
#9366=ORIENTED_EDGE('',*,*,#6895,.T.);
#9367=ORIENTED_EDGE('',*,*,#6849,.F.);
#9368=ORIENTED_EDGE('',*,*,#6883,.F.);
#9369=ORIENTED_EDGE('',*,*,#6822,.T.);
#9370=ORIENTED_EDGE('',*,*,#6811,.T.);
#9371=ORIENTED_EDGE('',*,*,#6816,.T.);
#9372=ORIENTED_EDGE('',*,*,#6809,.F.);
#9373=ORIENTED_EDGE('',*,*,#6863,.F.);
#9374=ORIENTED_EDGE('',*,*,#6875,.F.);
#9375=ORIENTED_EDGE('',*,*,#6904,.F.);
#9376=ORIENTED_EDGE('',*,*,#6884,.F.);
#9377=ORIENTED_EDGE('',*,*,#6902,.F.);
#9378=ORIENTED_EDGE('',*,*,#6878,.F.);
#9379=ORIENTED_EDGE('',*,*,#6867,.F.);
#9380=ORIENTED_EDGE('',*,*,#6853,.F.);
#9381=ORIENTED_EDGE('',*,*,#6901,.F.);
#9382=ORIENTED_EDGE('',*,*,#6856,.F.);
#9383=ORIENTED_EDGE('',*,*,#6866,.F.);
#9384=ORIENTED_EDGE('',*,*,#6889,.F.);
#9385=ORIENTED_EDGE('',*,*,#6859,.F.);
#9386=ORIENTED_EDGE('',*,*,#6887,.F.);
#9387=ORIENTED_EDGE('',*,*,#6903,.F.);
#9388=ORIENTED_EDGE('',*,*,#6892,.F.);
#9389=ORIENTED_EDGE('',*,*,#6907,.F.);
#9390=ORIENTED_EDGE('',*,*,#6908,.T.);
#9391=ORIENTED_EDGE('',*,*,#6909,.F.);
#9392=ORIENTED_EDGE('',*,*,#6908,.F.);
#9393=ORIENTED_EDGE('',*,*,#6910,.F.);
#9394=ORIENTED_EDGE('',*,*,#6911,.F.);
#9395=ORIENTED_EDGE('',*,*,#6912,.T.);
#9396=ORIENTED_EDGE('',*,*,#6913,.F.);
#9397=ORIENTED_EDGE('',*,*,#6912,.F.);
#9398=ORIENTED_EDGE('',*,*,#6910,.T.);
#9399=ORIENTED_EDGE('',*,*,#6911,.T.);
#9400=ORIENTED_EDGE('',*,*,#6914,.T.);
#9401=ORIENTED_EDGE('',*,*,#6907,.T.);
#9402=ORIENTED_EDGE('',*,*,#6914,.F.);
#9403=ORIENTED_EDGE('',*,*,#6909,.T.);
#9404=ORIENTED_EDGE('',*,*,#6913,.T.);
#9405=ORIENTED_EDGE('',*,*,#6915,.F.);
#9406=ORIENTED_EDGE('',*,*,#6916,.T.);
#9407=ORIENTED_EDGE('',*,*,#6917,.F.);
#9408=ORIENTED_EDGE('',*,*,#6916,.F.);
#9409=ORIENTED_EDGE('',*,*,#6918,.F.);
#9410=ORIENTED_EDGE('',*,*,#6919,.F.);
#9411=ORIENTED_EDGE('',*,*,#6920,.T.);
#9412=ORIENTED_EDGE('',*,*,#6921,.F.);
#9413=ORIENTED_EDGE('',*,*,#6920,.F.);
#9414=ORIENTED_EDGE('',*,*,#6918,.T.);
#9415=ORIENTED_EDGE('',*,*,#6919,.T.);
#9416=ORIENTED_EDGE('',*,*,#6922,.T.);
#9417=ORIENTED_EDGE('',*,*,#6915,.T.);
#9418=ORIENTED_EDGE('',*,*,#6922,.F.);
#9419=ORIENTED_EDGE('',*,*,#6917,.T.);
#9420=ORIENTED_EDGE('',*,*,#6921,.T.);
#9421=ORIENTED_EDGE('',*,*,#6923,.T.);
#9422=ORIENTED_EDGE('',*,*,#6924,.T.);
#9423=ORIENTED_EDGE('',*,*,#6925,.F.);
#9424=ORIENTED_EDGE('',*,*,#6924,.F.);
#9425=ORIENTED_EDGE('',*,*,#6926,.T.);
#9426=ORIENTED_EDGE('',*,*,#6927,.T.);
#9427=ORIENTED_EDGE('',*,*,#6928,.F.);
#9428=ORIENTED_EDGE('',*,*,#6927,.F.);
#9429=ORIENTED_EDGE('',*,*,#6929,.T.);
#9430=ORIENTED_EDGE('',*,*,#6930,.T.);
#9431=ORIENTED_EDGE('',*,*,#6931,.T.);
#9432=ORIENTED_EDGE('',*,*,#6932,.T.);
#9433=ORIENTED_EDGE('',*,*,#6933,.T.);
#9434=ORIENTED_EDGE('',*,*,#6934,.T.);
#9435=ORIENTED_EDGE('',*,*,#6935,.T.);
#9436=ORIENTED_EDGE('',*,*,#6936,.T.);
#9437=ORIENTED_EDGE('',*,*,#6923,.F.);
#9438=ORIENTED_EDGE('',*,*,#6926,.F.);
#9439=ORIENTED_EDGE('',*,*,#6937,.F.);
#9440=ORIENTED_EDGE('',*,*,#6938,.T.);
#9441=ORIENTED_EDGE('',*,*,#6939,.F.);
#9442=ORIENTED_EDGE('',*,*,#6940,.T.);
#9443=ORIENTED_EDGE('',*,*,#6941,.F.);
#9444=ORIENTED_EDGE('',*,*,#6942,.T.);
#9445=ORIENTED_EDGE('',*,*,#6943,.F.);
#9446=ORIENTED_EDGE('',*,*,#6944,.T.);
#9447=ORIENTED_EDGE('',*,*,#6928,.T.);
#9448=ORIENTED_EDGE('',*,*,#6925,.T.);
#9449=ORIENTED_EDGE('',*,*,#6931,.F.);
#9450=ORIENTED_EDGE('',*,*,#6945,.T.);
#9451=ORIENTED_EDGE('',*,*,#6937,.T.);
#9452=ORIENTED_EDGE('',*,*,#6946,.T.);
#9453=ORIENTED_EDGE('',*,*,#6933,.F.);
#9454=ORIENTED_EDGE('',*,*,#6947,.T.);
#9455=ORIENTED_EDGE('',*,*,#6943,.T.);
#9456=ORIENTED_EDGE('',*,*,#6948,.T.);
#9457=ORIENTED_EDGE('',*,*,#6941,.T.);
#9458=ORIENTED_EDGE('',*,*,#6949,.T.);
#9459=ORIENTED_EDGE('',*,*,#6935,.F.);
#9460=ORIENTED_EDGE('',*,*,#6950,.T.);
#9461=ORIENTED_EDGE('',*,*,#6939,.T.);
#9462=ORIENTED_EDGE('',*,*,#6951,.T.);
#9463=ORIENTED_EDGE('',*,*,#6929,.F.);
#9464=ORIENTED_EDGE('',*,*,#6952,.T.);
#9465=ORIENTED_EDGE('',*,*,#6930,.F.);
#9466=ORIENTED_EDGE('',*,*,#6951,.F.);
#9467=ORIENTED_EDGE('',*,*,#6938,.F.);
#9468=ORIENTED_EDGE('',*,*,#6945,.F.);
#9469=ORIENTED_EDGE('',*,*,#6932,.F.);
#9470=ORIENTED_EDGE('',*,*,#6946,.F.);
#9471=ORIENTED_EDGE('',*,*,#6944,.F.);
#9472=ORIENTED_EDGE('',*,*,#6947,.F.);
#9473=ORIENTED_EDGE('',*,*,#6936,.F.);
#9474=ORIENTED_EDGE('',*,*,#6949,.F.);
#9475=ORIENTED_EDGE('',*,*,#6940,.F.);
#9476=ORIENTED_EDGE('',*,*,#6952,.F.);
#9477=ORIENTED_EDGE('',*,*,#6934,.F.);
#9478=ORIENTED_EDGE('',*,*,#6948,.F.);
#9479=ORIENTED_EDGE('',*,*,#6942,.F.);
#9480=ORIENTED_EDGE('',*,*,#6950,.F.);
#9481=ORIENTED_EDGE('',*,*,#6953,.T.);
#9482=ORIENTED_EDGE('',*,*,#6954,.T.);
#9483=ORIENTED_EDGE('',*,*,#6955,.T.);
#9484=ORIENTED_EDGE('',*,*,#6954,.F.);
#9485=ORIENTED_EDGE('',*,*,#6956,.T.);
#9486=ORIENTED_EDGE('',*,*,#6957,.F.);
#9487=ORIENTED_EDGE('',*,*,#6958,.T.);
#9488=ORIENTED_EDGE('',*,*,#6959,.F.);
#9489=ORIENTED_EDGE('',*,*,#6960,.F.);
#9490=ORIENTED_EDGE('',*,*,#6958,.F.);
#9491=ORIENTED_EDGE('',*,*,#6961,.F.);
#9492=ORIENTED_EDGE('',*,*,#6962,.F.);
#9493=ORIENTED_EDGE('',*,*,#6963,.T.);
#9494=ORIENTED_EDGE('',*,*,#6964,.F.);
#9495=ORIENTED_EDGE('',*,*,#6963,.F.);
#9496=ORIENTED_EDGE('',*,*,#6965,.F.);
#9497=ORIENTED_EDGE('',*,*,#6966,.T.);
#9498=ORIENTED_EDGE('',*,*,#6967,.T.);
#9499=ORIENTED_EDGE('',*,*,#6966,.F.);
#9500=ORIENTED_EDGE('',*,*,#6968,.F.);
#9501=ORIENTED_EDGE('',*,*,#6969,.T.);
#9502=ORIENTED_EDGE('',*,*,#6970,.T.);
#9503=ORIENTED_EDGE('',*,*,#6969,.F.);
#9504=ORIENTED_EDGE('',*,*,#6953,.F.);
#9505=ORIENTED_EDGE('',*,*,#6956,.F.);
#9506=ORIENTED_EDGE('',*,*,#6971,.F.);
#9507=ORIENTED_EDGE('',*,*,#6972,.T.);
#9508=ORIENTED_EDGE('',*,*,#6973,.T.);
#9509=ORIENTED_EDGE('',*,*,#6972,.F.);
#9510=ORIENTED_EDGE('',*,*,#6974,.F.);
#9511=ORIENTED_EDGE('',*,*,#6975,.T.);
#9512=ORIENTED_EDGE('',*,*,#6976,.T.);
#9513=ORIENTED_EDGE('',*,*,#6975,.F.);
#9514=ORIENTED_EDGE('',*,*,#6977,.F.);
#9515=ORIENTED_EDGE('',*,*,#6978,.F.);
#9516=ORIENTED_EDGE('',*,*,#6979,.F.);
#9517=ORIENTED_EDGE('',*,*,#6980,.F.);
#9518=ORIENTED_EDGE('',*,*,#6981,.F.);
#9519=ORIENTED_EDGE('',*,*,#6982,.F.);
#9520=ORIENTED_EDGE('',*,*,#6983,.T.);
#9521=ORIENTED_EDGE('',*,*,#6984,.F.);
#9522=ORIENTED_EDGE('',*,*,#6985,.F.);
#9523=ORIENTED_EDGE('',*,*,#6986,.F.);
#9524=ORIENTED_EDGE('',*,*,#6987,.F.);
#9525=ORIENTED_EDGE('',*,*,#6988,.F.);
#9526=ORIENTED_EDGE('',*,*,#6989,.T.);
#9527=ORIENTED_EDGE('',*,*,#6990,.F.);
#9528=ORIENTED_EDGE('',*,*,#6991,.T.);
#9529=ORIENTED_EDGE('',*,*,#6992,.T.);
#9530=ORIENTED_EDGE('',*,*,#6993,.F.);
#9531=ORIENTED_EDGE('',*,*,#6994,.F.);
#9532=ORIENTED_EDGE('',*,*,#6995,.F.);
#9533=ORIENTED_EDGE('',*,*,#6996,.F.);
#9534=ORIENTED_EDGE('',*,*,#6997,.F.);
#9535=ORIENTED_EDGE('',*,*,#6998,.F.);
#9536=ORIENTED_EDGE('',*,*,#6992,.F.);
#9537=ORIENTED_EDGE('',*,*,#6999,.F.);
#9538=ORIENTED_EDGE('',*,*,#7000,.F.);
#9539=ORIENTED_EDGE('',*,*,#7001,.F.);
#9540=ORIENTED_EDGE('',*,*,#7002,.F.);
#9541=ORIENTED_EDGE('',*,*,#7003,.F.);
#9542=ORIENTED_EDGE('',*,*,#7004,.T.);
#9543=ORIENTED_EDGE('',*,*,#7005,.T.);
#9544=ORIENTED_EDGE('',*,*,#7004,.F.);
#9545=ORIENTED_EDGE('',*,*,#7006,.F.);
#9546=ORIENTED_EDGE('',*,*,#7007,.T.);
#9547=ORIENTED_EDGE('',*,*,#7008,.T.);
#9548=ORIENTED_EDGE('',*,*,#7007,.F.);
#9549=ORIENTED_EDGE('',*,*,#7009,.F.);
#9550=ORIENTED_EDGE('',*,*,#7010,.T.);
#9551=ORIENTED_EDGE('',*,*,#7011,.T.);
#9552=ORIENTED_EDGE('',*,*,#7010,.F.);
#9553=ORIENTED_EDGE('',*,*,#7012,.F.);
#9554=ORIENTED_EDGE('',*,*,#7013,.T.);
#9555=ORIENTED_EDGE('',*,*,#7014,.T.);
#9556=ORIENTED_EDGE('',*,*,#7015,.T.);
#9557=ORIENTED_EDGE('',*,*,#7016,.T.);
#9558=ORIENTED_EDGE('',*,*,#7013,.F.);
#9559=ORIENTED_EDGE('',*,*,#7017,.T.);
#9560=ORIENTED_EDGE('',*,*,#7018,.T.);
#9561=ORIENTED_EDGE('',*,*,#7014,.F.);
#9562=ORIENTED_EDGE('',*,*,#7019,.T.);
#9563=ORIENTED_EDGE('',*,*,#7020,.T.);
#9564=ORIENTED_EDGE('',*,*,#7021,.T.);
#9565=ORIENTED_EDGE('',*,*,#7022,.T.);
#9566=ORIENTED_EDGE('',*,*,#7023,.T.);
#9567=ORIENTED_EDGE('',*,*,#7024,.T.);
#9568=ORIENTED_EDGE('',*,*,#7019,.F.);
#9569=ORIENTED_EDGE('',*,*,#7016,.F.);
#9570=ORIENTED_EDGE('',*,*,#7025,.T.);
#9571=ORIENTED_EDGE('',*,*,#6961,.T.);
#9572=ORIENTED_EDGE('',*,*,#6962,.T.);
#9573=ORIENTED_EDGE('',*,*,#7026,.T.);
#9574=ORIENTED_EDGE('',*,*,#7027,.T.);
#9575=ORIENTED_EDGE('',*,*,#7028,.T.);
#9576=ORIENTED_EDGE('',*,*,#7029,.T.);
#9577=ORIENTED_EDGE('',*,*,#7030,.T.);
#9578=ORIENTED_EDGE('',*,*,#7031,.T.);
#9579=ORIENTED_EDGE('',*,*,#7032,.T.);
#9580=ORIENTED_EDGE('',*,*,#6959,.T.);
#9581=ORIENTED_EDGE('',*,*,#6960,.T.);
#9582=ORIENTED_EDGE('',*,*,#7032,.F.);
#9583=ORIENTED_EDGE('',*,*,#7033,.T.);
#9584=ORIENTED_EDGE('',*,*,#7034,.F.);
#9585=ORIENTED_EDGE('',*,*,#7035,.T.);
#9586=ORIENTED_EDGE('',*,*,#7036,.F.);
#9587=ORIENTED_EDGE('',*,*,#7037,.T.);
#9588=ORIENTED_EDGE('',*,*,#7026,.F.);
#9589=ORIENTED_EDGE('',*,*,#7038,.T.);
#9590=ORIENTED_EDGE('',*,*,#7039,.T.);
#9591=ORIENTED_EDGE('',*,*,#7040,.T.);
#9592=ORIENTED_EDGE('',*,*,#7041,.T.);
#9593=ORIENTED_EDGE('',*,*,#6991,.F.);
#9594=ORIENTED_EDGE('',*,*,#7042,.T.);
#9595=ORIENTED_EDGE('',*,*,#7043,.T.);
#9596=ORIENTED_EDGE('',*,*,#7029,.F.);
#9597=ORIENTED_EDGE('',*,*,#7044,.T.);
#9598=ORIENTED_EDGE('',*,*,#7045,.T.);
#9599=ORIENTED_EDGE('',*,*,#7046,.T.);
#9600=ORIENTED_EDGE('',*,*,#7042,.F.);
#9601=ORIENTED_EDGE('',*,*,#7047,.T.);
#9602=ORIENTED_EDGE('',*,*,#6957,.T.);
#9603=ORIENTED_EDGE('',*,*,#6976,.F.);
#9604=ORIENTED_EDGE('',*,*,#6964,.T.);
#9605=ORIENTED_EDGE('',*,*,#6974,.T.);
#9606=ORIENTED_EDGE('',*,*,#7024,.F.);
#9607=ORIENTED_EDGE('',*,*,#7048,.T.);
#9608=ORIENTED_EDGE('',*,*,#7045,.F.);
#9609=ORIENTED_EDGE('',*,*,#7049,.T.);
#9610=ORIENTED_EDGE('',*,*,#7020,.F.);
#9611=ORIENTED_EDGE('',*,*,#7038,.F.);
#9612=ORIENTED_EDGE('',*,*,#7050,.T.);
#9613=ORIENTED_EDGE('',*,*,#7022,.F.);
#9614=ORIENTED_EDGE('',*,*,#7051,.T.);
#9615=ORIENTED_EDGE('',*,*,#7012,.T.);
#9616=ORIENTED_EDGE('',*,*,#7011,.F.);
#9617=ORIENTED_EDGE('',*,*,#7009,.T.);
#9618=ORIENTED_EDGE('',*,*,#7008,.F.);
#9619=ORIENTED_EDGE('',*,*,#7006,.T.);
#9620=ORIENTED_EDGE('',*,*,#7005,.F.);
#9621=ORIENTED_EDGE('',*,*,#7003,.T.);
#9622=ORIENTED_EDGE('',*,*,#7052,.F.);
#9623=ORIENTED_EDGE('',*,*,#7053,.F.);
#9624=ORIENTED_EDGE('',*,*,#7054,.F.);
#9625=ORIENTED_EDGE('',*,*,#7055,.F.);
#9626=ORIENTED_EDGE('',*,*,#7056,.F.);
#9627=ORIENTED_EDGE('',*,*,#7057,.F.);
#9628=ORIENTED_EDGE('',*,*,#7058,.F.);
#9629=ORIENTED_EDGE('',*,*,#7059,.T.);
#9630=ORIENTED_EDGE('',*,*,#7060,.T.);
#9631=ORIENTED_EDGE('',*,*,#7052,.T.);
#9632=ORIENTED_EDGE('',*,*,#7061,.F.);
#9633=ORIENTED_EDGE('',*,*,#7062,.T.);
#9634=ORIENTED_EDGE('',*,*,#7058,.T.);
#9635=ORIENTED_EDGE('',*,*,#7057,.T.);
#9636=ORIENTED_EDGE('',*,*,#7063,.F.);
#9637=ORIENTED_EDGE('',*,*,#7064,.T.);
#9638=ORIENTED_EDGE('',*,*,#7061,.T.);
#9639=ORIENTED_EDGE('',*,*,#7056,.T.);
#9640=ORIENTED_EDGE('',*,*,#7065,.F.);
#9641=ORIENTED_EDGE('',*,*,#7066,.T.);
#9642=ORIENTED_EDGE('',*,*,#7063,.T.);
#9643=ORIENTED_EDGE('',*,*,#7055,.T.);
#9644=ORIENTED_EDGE('',*,*,#7067,.F.);
#9645=ORIENTED_EDGE('',*,*,#7068,.T.);
#9646=ORIENTED_EDGE('',*,*,#7065,.T.);
#9647=ORIENTED_EDGE('',*,*,#7054,.T.);
#9648=ORIENTED_EDGE('',*,*,#7060,.F.);
#9649=ORIENTED_EDGE('',*,*,#7069,.T.);
#9650=ORIENTED_EDGE('',*,*,#7067,.T.);
#9651=ORIENTED_EDGE('',*,*,#7053,.T.);
#9652=ORIENTED_EDGE('',*,*,#7070,.T.);
#9653=ORIENTED_EDGE('',*,*,#7071,.T.);
#9654=ORIENTED_EDGE('',*,*,#7072,.T.);
#9655=ORIENTED_EDGE('',*,*,#7073,.T.);
#9656=ORIENTED_EDGE('',*,*,#7074,.T.);
#9657=ORIENTED_EDGE('',*,*,#7075,.T.);
#9658=ORIENTED_EDGE('',*,*,#6967,.F.);
#9659=ORIENTED_EDGE('',*,*,#7076,.F.);
#9660=ORIENTED_EDGE('',*,*,#7077,.F.);
#9661=ORIENTED_EDGE('',*,*,#7078,.F.);
#9662=ORIENTED_EDGE('',*,*,#7079,.T.);
#9663=ORIENTED_EDGE('',*,*,#7080,.T.);
#9664=ORIENTED_EDGE('',*,*,#7000,.T.);
#9665=ORIENTED_EDGE('',*,*,#7081,.T.);
#9666=ORIENTED_EDGE('',*,*,#7082,.T.);
#9667=ORIENTED_EDGE('',*,*,#7015,.F.);
#9668=ORIENTED_EDGE('',*,*,#7083,.T.);
#9669=ORIENTED_EDGE('',*,*,#7079,.F.);
#9670=ORIENTED_EDGE('',*,*,#7084,.F.);
#9671=ORIENTED_EDGE('',*,*,#7085,.F.);
#9672=ORIENTED_EDGE('',*,*,#7086,.T.);
#9673=ORIENTED_EDGE('',*,*,#7082,.F.);
#9674=ORIENTED_EDGE('',*,*,#7087,.F.);
#9675=ORIENTED_EDGE('',*,*,#7081,.F.);
#9676=ORIENTED_EDGE('',*,*,#6999,.T.);
#9677=ORIENTED_EDGE('',*,*,#7088,.F.);
#9678=ORIENTED_EDGE('',*,*,#7025,.F.);
#9679=ORIENTED_EDGE('',*,*,#7087,.T.);
#9680=ORIENTED_EDGE('',*,*,#6973,.F.);
#9681=ORIENTED_EDGE('',*,*,#7089,.T.);
#9682=ORIENTED_EDGE('',*,*,#7001,.T.);
#9683=ORIENTED_EDGE('',*,*,#7080,.F.);
#9684=ORIENTED_EDGE('',*,*,#7083,.F.);
#9685=ORIENTED_EDGE('',*,*,#7018,.F.);
#9686=ORIENTED_EDGE('',*,*,#6971,.T.);
#9687=ORIENTED_EDGE('',*,*,#7088,.T.);
#9688=ORIENTED_EDGE('',*,*,#7002,.T.);
#9689=ORIENTED_EDGE('',*,*,#7089,.F.);
#9690=ORIENTED_EDGE('',*,*,#7017,.F.);
#9691=ORIENTED_EDGE('',*,*,#7090,.F.);
#9692=ORIENTED_EDGE('',*,*,#7091,.T.);
#9693=ORIENTED_EDGE('',*,*,#7092,.F.);
#9694=ORIENTED_EDGE('',*,*,#7084,.T.);
#9695=ORIENTED_EDGE('',*,*,#7078,.T.);
#9696=ORIENTED_EDGE('',*,*,#7093,.F.);
#9697=ORIENTED_EDGE('',*,*,#7094,.T.);
#9698=ORIENTED_EDGE('',*,*,#7090,.T.);
#9699=ORIENTED_EDGE('',*,*,#7077,.T.);
#9700=ORIENTED_EDGE('',*,*,#7095,.F.);
#9701=ORIENTED_EDGE('',*,*,#7096,.T.);
#9702=ORIENTED_EDGE('',*,*,#7093,.T.);
#9703=ORIENTED_EDGE('',*,*,#7076,.T.);
#9704=ORIENTED_EDGE('',*,*,#7086,.F.);
#9705=ORIENTED_EDGE('',*,*,#7092,.T.);
#9706=ORIENTED_EDGE('',*,*,#7097,.T.);
#9707=ORIENTED_EDGE('',*,*,#7095,.T.);
#9708=ORIENTED_EDGE('',*,*,#7085,.T.);
#9709=ORIENTED_EDGE('',*,*,#7098,.F.);
#9710=ORIENTED_EDGE('',*,*,#6998,.T.);
#9711=ORIENTED_EDGE('',*,*,#7099,.F.);
#9712=ORIENTED_EDGE('',*,*,#7100,.F.);
#9713=ORIENTED_EDGE('',*,*,#6997,.T.);
#9714=ORIENTED_EDGE('',*,*,#7101,.F.);
#9715=ORIENTED_EDGE('',*,*,#7102,.F.);
#9716=ORIENTED_EDGE('',*,*,#6996,.T.);
#9717=ORIENTED_EDGE('',*,*,#7103,.F.);
#9718=ORIENTED_EDGE('',*,*,#7104,.F.);
#9719=ORIENTED_EDGE('',*,*,#6995,.T.);
#9720=ORIENTED_EDGE('',*,*,#7105,.F.);
#9721=ORIENTED_EDGE('',*,*,#7106,.F.);
#9722=ORIENTED_EDGE('',*,*,#6994,.T.);
#9723=ORIENTED_EDGE('',*,*,#7107,.F.);
#9724=ORIENTED_EDGE('',*,*,#7108,.F.);
#9725=ORIENTED_EDGE('',*,*,#6993,.T.);
#9726=ORIENTED_EDGE('',*,*,#7109,.F.);
#9727=ORIENTED_EDGE('',*,*,#7110,.T.);
#9728=ORIENTED_EDGE('',*,*,#7111,.T.);
#9729=ORIENTED_EDGE('',*,*,#7112,.T.);
#9730=ORIENTED_EDGE('',*,*,#7105,.T.);
#9731=ORIENTED_EDGE('',*,*,#7106,.T.);
#9732=ORIENTED_EDGE('',*,*,#7113,.F.);
#9733=ORIENTED_EDGE('',*,*,#6980,.T.);
#9734=ORIENTED_EDGE('',*,*,#7114,.T.);
#9735=ORIENTED_EDGE('',*,*,#6981,.T.);
#9736=ORIENTED_EDGE('',*,*,#7113,.T.);
#9737=ORIENTED_EDGE('',*,*,#7107,.T.);
#9738=ORIENTED_EDGE('',*,*,#7108,.T.);
#9739=ORIENTED_EDGE('',*,*,#7115,.F.);
#9740=ORIENTED_EDGE('',*,*,#7116,.T.);
#9741=ORIENTED_EDGE('',*,*,#7117,.T.);
#9742=ORIENTED_EDGE('',*,*,#7118,.T.);
#9743=ORIENTED_EDGE('',*,*,#7115,.T.);
#9744=ORIENTED_EDGE('',*,*,#7109,.T.);
#9745=ORIENTED_EDGE('',*,*,#7098,.T.);
#9746=ORIENTED_EDGE('',*,*,#7119,.F.);
#9747=ORIENTED_EDGE('',*,*,#7120,.T.);
#9748=ORIENTED_EDGE('',*,*,#7121,.T.);
#9749=ORIENTED_EDGE('',*,*,#7122,.T.);
#9750=ORIENTED_EDGE('',*,*,#7119,.T.);
#9751=ORIENTED_EDGE('',*,*,#7099,.T.);
#9752=ORIENTED_EDGE('',*,*,#7100,.T.);
#9753=ORIENTED_EDGE('',*,*,#7123,.F.);
#9754=ORIENTED_EDGE('',*,*,#6984,.T.);
#9755=ORIENTED_EDGE('',*,*,#7124,.F.);
#9756=ORIENTED_EDGE('',*,*,#7125,.T.);
#9757=ORIENTED_EDGE('',*,*,#7126,.T.);
#9758=ORIENTED_EDGE('',*,*,#6985,.T.);
#9759=ORIENTED_EDGE('',*,*,#7123,.T.);
#9760=ORIENTED_EDGE('',*,*,#7101,.T.);
#9761=ORIENTED_EDGE('',*,*,#7102,.T.);
#9762=ORIENTED_EDGE('',*,*,#7112,.F.);
#9763=ORIENTED_EDGE('',*,*,#7127,.T.);
#9764=ORIENTED_EDGE('',*,*,#7128,.T.);
#9765=ORIENTED_EDGE('',*,*,#7129,.T.);
#9766=ORIENTED_EDGE('',*,*,#7124,.T.);
#9767=ORIENTED_EDGE('',*,*,#7103,.T.);
#9768=ORIENTED_EDGE('',*,*,#7104,.T.);
#9769=ORIENTED_EDGE('',*,*,#7130,.T.);
#9770=ORIENTED_EDGE('',*,*,#7131,.T.);
#9771=ORIENTED_EDGE('',*,*,#6977,.T.);
#9772=ORIENTED_EDGE('',*,*,#7132,.T.);
#9773=ORIENTED_EDGE('',*,*,#7133,.T.);
#9774=ORIENTED_EDGE('',*,*,#6988,.T.);
#9775=ORIENTED_EDGE('',*,*,#6970,.F.);
#9776=ORIENTED_EDGE('',*,*,#6979,.T.);
#9777=ORIENTED_EDGE('',*,*,#7134,.T.);
#9778=ORIENTED_EDGE('',*,*,#7110,.F.);
#9779=ORIENTED_EDGE('',*,*,#7135,.T.);
#9780=ORIENTED_EDGE('',*,*,#6982,.T.);
#9781=ORIENTED_EDGE('',*,*,#7114,.F.);
#9782=ORIENTED_EDGE('',*,*,#7128,.F.);
#9783=ORIENTED_EDGE('',*,*,#7136,.T.);
#9784=ORIENTED_EDGE('',*,*,#7137,.T.);
#9785=ORIENTED_EDGE('',*,*,#7138,.T.);
#9786=ORIENTED_EDGE('',*,*,#7139,.T.);
#9787=ORIENTED_EDGE('',*,*,#7117,.F.);
#9788=ORIENTED_EDGE('',*,*,#7126,.F.);
#9789=ORIENTED_EDGE('',*,*,#7140,.T.);
#9790=ORIENTED_EDGE('',*,*,#6986,.T.);
#9791=ORIENTED_EDGE('',*,*,#6990,.T.);
#9792=ORIENTED_EDGE('',*,*,#7141,.T.);
#9793=ORIENTED_EDGE('',*,*,#7121,.F.);
#9794=ORIENTED_EDGE('',*,*,#6989,.F.);
#9795=ORIENTED_EDGE('',*,*,#7133,.F.);
#9796=ORIENTED_EDGE('',*,*,#7142,.F.);
#9797=ORIENTED_EDGE('',*,*,#7138,.F.);
#9798=ORIENTED_EDGE('',*,*,#7120,.F.);
#9799=ORIENTED_EDGE('',*,*,#7122,.F.);
#9800=ORIENTED_EDGE('',*,*,#7141,.F.);
#9801=ORIENTED_EDGE('',*,*,#7142,.T.);
#9802=ORIENTED_EDGE('',*,*,#7132,.F.);
#9803=ORIENTED_EDGE('',*,*,#6983,.F.);
#9804=ORIENTED_EDGE('',*,*,#7135,.F.);
#9805=ORIENTED_EDGE('',*,*,#7116,.F.);
#9806=ORIENTED_EDGE('',*,*,#7118,.F.);
#9807=ORIENTED_EDGE('',*,*,#7139,.F.);
#9808=ORIENTED_EDGE('',*,*,#7129,.F.);
#9809=ORIENTED_EDGE('',*,*,#7137,.F.);
#9810=ORIENTED_EDGE('',*,*,#7143,.F.);
#9811=ORIENTED_EDGE('',*,*,#7130,.F.);
#9812=ORIENTED_EDGE('',*,*,#6987,.T.);
#9813=ORIENTED_EDGE('',*,*,#7140,.F.);
#9814=ORIENTED_EDGE('',*,*,#7125,.F.);
#9815=ORIENTED_EDGE('',*,*,#7134,.F.);
#9816=ORIENTED_EDGE('',*,*,#6978,.T.);
#9817=ORIENTED_EDGE('',*,*,#7131,.F.);
#9818=ORIENTED_EDGE('',*,*,#7143,.T.);
#9819=ORIENTED_EDGE('',*,*,#7136,.F.);
#9820=ORIENTED_EDGE('',*,*,#7127,.F.);
#9821=ORIENTED_EDGE('',*,*,#7111,.F.);
#9822=ORIENTED_EDGE('',*,*,#7144,.T.);
#9823=ORIENTED_EDGE('',*,*,#7145,.T.);
#9824=ORIENTED_EDGE('',*,*,#7023,.F.);
#9825=ORIENTED_EDGE('',*,*,#7146,.T.);
#9826=ORIENTED_EDGE('',*,*,#7147,.T.);
#9827=ORIENTED_EDGE('',*,*,#7021,.F.);
#9828=ORIENTED_EDGE('',*,*,#7148,.T.);
#9829=ORIENTED_EDGE('',*,*,#7149,.T.);
#9830=ORIENTED_EDGE('',*,*,#7150,.T.);
#9831=ORIENTED_EDGE('',*,*,#7151,.T.);
#9832=ORIENTED_EDGE('',*,*,#6968,.T.);
#9833=ORIENTED_EDGE('',*,*,#6965,.T.);
#9834=ORIENTED_EDGE('',*,*,#6955,.F.);
#9835=ORIENTED_EDGE('',*,*,#7049,.F.);
#9836=ORIENTED_EDGE('',*,*,#7047,.F.);
#9837=ORIENTED_EDGE('',*,*,#7152,.F.);
#9838=ORIENTED_EDGE('',*,*,#7148,.F.);
#9839=ORIENTED_EDGE('',*,*,#7152,.T.);
#9840=ORIENTED_EDGE('',*,*,#7044,.F.);
#9841=ORIENTED_EDGE('',*,*,#7153,.F.);
#9842=ORIENTED_EDGE('',*,*,#7149,.F.);
#9843=ORIENTED_EDGE('',*,*,#7153,.T.);
#9844=ORIENTED_EDGE('',*,*,#7028,.F.);
#9845=ORIENTED_EDGE('',*,*,#7154,.F.);
#9846=ORIENTED_EDGE('',*,*,#7154,.T.);
#9847=ORIENTED_EDGE('',*,*,#7027,.F.);
#9848=ORIENTED_EDGE('',*,*,#7037,.F.);
#9849=ORIENTED_EDGE('',*,*,#7155,.F.);
#9850=ORIENTED_EDGE('',*,*,#7150,.F.);
#9851=ORIENTED_EDGE('',*,*,#7051,.F.);
#9852=ORIENTED_EDGE('',*,*,#7151,.F.);
#9853=ORIENTED_EDGE('',*,*,#7156,.F.);
#9854=ORIENTED_EDGE('',*,*,#7039,.F.);
#9855=ORIENTED_EDGE('',*,*,#7155,.T.);
#9856=ORIENTED_EDGE('',*,*,#7036,.T.);
#9857=ORIENTED_EDGE('',*,*,#7157,.F.);
#9858=ORIENTED_EDGE('',*,*,#7156,.T.);
#9859=ORIENTED_EDGE('',*,*,#7048,.F.);
#9860=ORIENTED_EDGE('',*,*,#7145,.F.);
#9861=ORIENTED_EDGE('',*,*,#7158,.F.);
#9862=ORIENTED_EDGE('',*,*,#7046,.F.);
#9863=ORIENTED_EDGE('',*,*,#7157,.T.);
#9864=ORIENTED_EDGE('',*,*,#7035,.F.);
#9865=ORIENTED_EDGE('',*,*,#7159,.F.);
#9866=ORIENTED_EDGE('',*,*,#7040,.F.);
#9867=ORIENTED_EDGE('',*,*,#7050,.F.);
#9868=ORIENTED_EDGE('',*,*,#7041,.F.);
#9869=ORIENTED_EDGE('',*,*,#7160,.F.);
#9870=ORIENTED_EDGE('',*,*,#7146,.F.);
#9871=ORIENTED_EDGE('',*,*,#7158,.T.);
#9872=ORIENTED_EDGE('',*,*,#7144,.F.);
#9873=ORIENTED_EDGE('',*,*,#7161,.F.);
#9874=ORIENTED_EDGE('',*,*,#7043,.F.);
#9875=ORIENTED_EDGE('',*,*,#7159,.T.);
#9876=ORIENTED_EDGE('',*,*,#7034,.T.);
#9877=ORIENTED_EDGE('',*,*,#7162,.F.);
#9878=ORIENTED_EDGE('',*,*,#7160,.T.);
#9879=ORIENTED_EDGE('',*,*,#7030,.F.);
#9880=ORIENTED_EDGE('',*,*,#7161,.T.);
#9881=ORIENTED_EDGE('',*,*,#7163,.F.);
#9882=ORIENTED_EDGE('',*,*,#7162,.T.);
#9883=ORIENTED_EDGE('',*,*,#7033,.F.);
#9884=ORIENTED_EDGE('',*,*,#7031,.F.);
#9885=ORIENTED_EDGE('',*,*,#7163,.T.);
#9886=ORIENTED_EDGE('',*,*,#7147,.F.);
#9887=ORIENTED_EDGE('',*,*,#7164,.F.);
#9888=ORIENTED_EDGE('',*,*,#7064,.F.);
#9889=ORIENTED_EDGE('',*,*,#7165,.F.);
#9890=ORIENTED_EDGE('',*,*,#7074,.F.);
#9891=ORIENTED_EDGE('',*,*,#7165,.T.);
#9892=ORIENTED_EDGE('',*,*,#7066,.F.);
#9893=ORIENTED_EDGE('',*,*,#7166,.F.);
#9894=ORIENTED_EDGE('',*,*,#7075,.F.);
#9895=ORIENTED_EDGE('',*,*,#7164,.T.);
#9896=ORIENTED_EDGE('',*,*,#7073,.F.);
#9897=ORIENTED_EDGE('',*,*,#7167,.F.);
#9898=ORIENTED_EDGE('',*,*,#7062,.F.);
#9899=ORIENTED_EDGE('',*,*,#7166,.T.);
#9900=ORIENTED_EDGE('',*,*,#7068,.F.);
#9901=ORIENTED_EDGE('',*,*,#7168,.F.);
#9902=ORIENTED_EDGE('',*,*,#7070,.F.);
#9903=ORIENTED_EDGE('',*,*,#7167,.T.);
#9904=ORIENTED_EDGE('',*,*,#7072,.F.);
#9905=ORIENTED_EDGE('',*,*,#7169,.F.);
#9906=ORIENTED_EDGE('',*,*,#7059,.F.);
#9907=ORIENTED_EDGE('',*,*,#7168,.T.);
#9908=ORIENTED_EDGE('',*,*,#7069,.F.);
#9909=ORIENTED_EDGE('',*,*,#7169,.T.);
#9910=ORIENTED_EDGE('',*,*,#7071,.F.);
#9911=ORIENTED_EDGE('',*,*,#7091,.F.);
#9912=ORIENTED_EDGE('',*,*,#7094,.F.);
#9913=ORIENTED_EDGE('',*,*,#7096,.F.);
#9914=ORIENTED_EDGE('',*,*,#7097,.F.);
#9915=ORIENTED_EDGE('',*,*,#7170,.F.);
#9916=ORIENTED_EDGE('',*,*,#7171,.F.);
#9917=ORIENTED_EDGE('',*,*,#7172,.F.);
#9918=ORIENTED_EDGE('',*,*,#7173,.T.);
#9919=ORIENTED_EDGE('',*,*,#7174,.F.);
#9920=ORIENTED_EDGE('',*,*,#7173,.F.);
#9921=ORIENTED_EDGE('',*,*,#7175,.F.);
#9922=ORIENTED_EDGE('',*,*,#7176,.F.);
#9923=ORIENTED_EDGE('',*,*,#7176,.T.);
#9924=ORIENTED_EDGE('',*,*,#7177,.F.);
#9925=ORIENTED_EDGE('',*,*,#7178,.T.);
#9926=ORIENTED_EDGE('',*,*,#7179,.F.);
#9927=ORIENTED_EDGE('',*,*,#7178,.F.);
#9928=ORIENTED_EDGE('',*,*,#7180,.F.);
#9929=ORIENTED_EDGE('',*,*,#7181,.T.);
#9930=ORIENTED_EDGE('',*,*,#7182,.T.);
#9931=ORIENTED_EDGE('',*,*,#7183,.F.);
#9932=ORIENTED_EDGE('',*,*,#7171,.T.);
#9933=ORIENTED_EDGE('',*,*,#7184,.F.);
#9934=ORIENTED_EDGE('',*,*,#7182,.F.);
#9935=ORIENTED_EDGE('',*,*,#7185,.T.);
#9936=ORIENTED_EDGE('',*,*,#7186,.T.);
#9937=ORIENTED_EDGE('',*,*,#7187,.T.);
#9938=ORIENTED_EDGE('',*,*,#7188,.T.);
#9939=ORIENTED_EDGE('',*,*,#7186,.F.);
#9940=ORIENTED_EDGE('',*,*,#7189,.T.);
#9941=ORIENTED_EDGE('',*,*,#7190,.T.);
#9942=ORIENTED_EDGE('',*,*,#7191,.T.);
#9943=ORIENTED_EDGE('',*,*,#7187,.F.);
#9944=ORIENTED_EDGE('',*,*,#7188,.F.);
#9945=ORIENTED_EDGE('',*,*,#7191,.F.);
#9946=ORIENTED_EDGE('',*,*,#7185,.F.);
#9947=ORIENTED_EDGE('',*,*,#7192,.T.);
#9948=ORIENTED_EDGE('',*,*,#7172,.T.);
#9949=ORIENTED_EDGE('',*,*,#7183,.T.);
#9950=ORIENTED_EDGE('',*,*,#7184,.T.);
#9951=ORIENTED_EDGE('',*,*,#7170,.T.);
#9952=ORIENTED_EDGE('',*,*,#7180,.T.);
#9953=ORIENTED_EDGE('',*,*,#7177,.T.);
#9954=ORIENTED_EDGE('',*,*,#7175,.T.);
#9955=ORIENTED_EDGE('',*,*,#7192,.F.);
#9956=ORIENTED_EDGE('',*,*,#7189,.F.);
#9957=ORIENTED_EDGE('',*,*,#7190,.F.);
#9958=ORIENTED_EDGE('',*,*,#7174,.T.);
#9959=ORIENTED_EDGE('',*,*,#7181,.F.);
#9960=ORIENTED_EDGE('',*,*,#7179,.T.);
#9961=ORIENTED_EDGE('',*,*,#7193,.F.);
#9962=ORIENTED_EDGE('',*,*,#7194,.T.);
#9963=ORIENTED_EDGE('',*,*,#7195,.T.);
#9964=ORIENTED_EDGE('',*,*,#7194,.F.);
#9965=ORIENTED_EDGE('',*,*,#7196,.F.);
#9966=ORIENTED_EDGE('',*,*,#7197,.T.);
#9967=ORIENTED_EDGE('',*,*,#7198,.T.);
#9968=ORIENTED_EDGE('',*,*,#7197,.F.);
#9969=ORIENTED_EDGE('',*,*,#7199,.F.);
#9970=ORIENTED_EDGE('',*,*,#7200,.T.);
#9971=ORIENTED_EDGE('',*,*,#7201,.T.);
#9972=ORIENTED_EDGE('',*,*,#7200,.F.);
#9973=ORIENTED_EDGE('',*,*,#7202,.F.);
#9974=ORIENTED_EDGE('',*,*,#7203,.T.);
#9975=ORIENTED_EDGE('',*,*,#7204,.T.);
#9976=ORIENTED_EDGE('',*,*,#7203,.F.);
#9977=ORIENTED_EDGE('',*,*,#7205,.F.);
#9978=ORIENTED_EDGE('',*,*,#7206,.T.);
#9979=ORIENTED_EDGE('',*,*,#7207,.T.);
#9980=ORIENTED_EDGE('',*,*,#7206,.F.);
#9981=ORIENTED_EDGE('',*,*,#7207,.F.);
#9982=ORIENTED_EDGE('',*,*,#7205,.T.);
#9983=ORIENTED_EDGE('',*,*,#7204,.F.);
#9984=ORIENTED_EDGE('',*,*,#7201,.F.);
#9985=ORIENTED_EDGE('',*,*,#7202,.T.);
#9986=ORIENTED_EDGE('',*,*,#7199,.T.);
#9987=ORIENTED_EDGE('',*,*,#7198,.F.);
#9988=ORIENTED_EDGE('',*,*,#7195,.F.);
#9989=ORIENTED_EDGE('',*,*,#7196,.T.);
#9990=ORIENTED_EDGE('',*,*,#7193,.T.);
#9991=ORIENTED_EDGE('',*,*,#7208,.F.);
#9992=ORIENTED_EDGE('',*,*,#7209,.T.);
#9993=ORIENTED_EDGE('',*,*,#7208,.T.);
#9994=ORIENTED_EDGE('',*,*,#7209,.F.);
#9995=ORIENTED_EDGE('',*,*,#7210,.F.);
#9996=ORIENTED_EDGE('',*,*,#7211,.T.);
#9997=ORIENTED_EDGE('',*,*,#7212,.T.);
#9998=ORIENTED_EDGE('',*,*,#7213,.F.);
#9999=ORIENTED_EDGE('',*,*,#7214,.F.);
#10000=ORIENTED_EDGE('',*,*,#7215,.T.);
#10001=ORIENTED_EDGE('',*,*,#7216,.F.);
#10002=ORIENTED_EDGE('',*,*,#7217,.F.);
#10003=ORIENTED_EDGE('',*,*,#7218,.F.);
#10004=ORIENTED_EDGE('',*,*,#7219,.T.);
#10005=ORIENTED_EDGE('',*,*,#7220,.F.);
#10006=ORIENTED_EDGE('',*,*,#7221,.F.);
#10007=ORIENTED_EDGE('',*,*,#7222,.F.);
#10008=ORIENTED_EDGE('',*,*,#7223,.T.);
#10009=ORIENTED_EDGE('',*,*,#7224,.T.);
#10010=ORIENTED_EDGE('',*,*,#7225,.T.);
#10011=ORIENTED_EDGE('',*,*,#7224,.F.);
#10012=ORIENTED_EDGE('',*,*,#7226,.T.);
#10013=ORIENTED_EDGE('',*,*,#7214,.T.);
#10014=ORIENTED_EDGE('',*,*,#7227,.T.);
#10015=ORIENTED_EDGE('',*,*,#7228,.T.);
#10016=ORIENTED_EDGE('',*,*,#7229,.T.);
#10017=ORIENTED_EDGE('',*,*,#7230,.T.);
#10018=ORIENTED_EDGE('',*,*,#7231,.T.);
#10019=ORIENTED_EDGE('',*,*,#7232,.T.);
#10020=ORIENTED_EDGE('',*,*,#7233,.T.);
#10021=ORIENTED_EDGE('',*,*,#7234,.T.);
#10022=ORIENTED_EDGE('',*,*,#7235,.T.);
#10023=ORIENTED_EDGE('',*,*,#7236,.F.);
#10024=ORIENTED_EDGE('',*,*,#7237,.F.);
#10025=ORIENTED_EDGE('',*,*,#7238,.F.);
#10026=ORIENTED_EDGE('',*,*,#7239,.F.);
#10027=ORIENTED_EDGE('',*,*,#7240,.F.);
#10028=ORIENTED_EDGE('',*,*,#7241,.F.);
#10029=ORIENTED_EDGE('',*,*,#7242,.F.);
#10030=ORIENTED_EDGE('',*,*,#7243,.F.);
#10031=ORIENTED_EDGE('',*,*,#7244,.T.);
#10032=ORIENTED_EDGE('',*,*,#7245,.T.);
#10033=ORIENTED_EDGE('',*,*,#7246,.F.);
#10034=ORIENTED_EDGE('',*,*,#7247,.F.);
#10035=ORIENTED_EDGE('',*,*,#7248,.F.);
#10036=ORIENTED_EDGE('',*,*,#7249,.F.);
#10037=ORIENTED_EDGE('',*,*,#7250,.F.);
#10038=ORIENTED_EDGE('',*,*,#7251,.F.);
#10039=ORIENTED_EDGE('',*,*,#7252,.F.);
#10040=ORIENTED_EDGE('',*,*,#7253,.F.);
#10041=ORIENTED_EDGE('',*,*,#7212,.F.);
#10042=ORIENTED_EDGE('',*,*,#7254,.T.);
#10043=ORIENTED_EDGE('',*,*,#7218,.T.);
#10044=ORIENTED_EDGE('',*,*,#7255,.T.);
#10045=ORIENTED_EDGE('',*,*,#7256,.T.);
#10046=ORIENTED_EDGE('',*,*,#7257,.T.);
#10047=ORIENTED_EDGE('',*,*,#7258,.T.);
#10048=ORIENTED_EDGE('',*,*,#7259,.T.);
#10049=ORIENTED_EDGE('',*,*,#7260,.T.);
#10050=ORIENTED_EDGE('',*,*,#7261,.T.);
#10051=ORIENTED_EDGE('',*,*,#7253,.T.);
#10052=ORIENTED_EDGE('',*,*,#7262,.F.);
#10053=ORIENTED_EDGE('',*,*,#7227,.F.);
#10054=ORIENTED_EDGE('',*,*,#7213,.T.);
#10055=ORIENTED_EDGE('',*,*,#7252,.T.);
#10056=ORIENTED_EDGE('',*,*,#7263,.F.);
#10057=ORIENTED_EDGE('',*,*,#7228,.F.);
#10058=ORIENTED_EDGE('',*,*,#7262,.T.);
#10059=ORIENTED_EDGE('',*,*,#7251,.T.);
#10060=ORIENTED_EDGE('',*,*,#7264,.F.);
#10061=ORIENTED_EDGE('',*,*,#7229,.F.);
#10062=ORIENTED_EDGE('',*,*,#7263,.T.);
#10063=ORIENTED_EDGE('',*,*,#7250,.T.);
#10064=ORIENTED_EDGE('',*,*,#7265,.F.);
#10065=ORIENTED_EDGE('',*,*,#7230,.F.);
#10066=ORIENTED_EDGE('',*,*,#7264,.T.);
#10067=ORIENTED_EDGE('',*,*,#7249,.T.);
#10068=ORIENTED_EDGE('',*,*,#7266,.F.);
#10069=ORIENTED_EDGE('',*,*,#7231,.F.);
#10070=ORIENTED_EDGE('',*,*,#7265,.T.);
#10071=ORIENTED_EDGE('',*,*,#7248,.T.);
#10072=ORIENTED_EDGE('',*,*,#7267,.F.);
#10073=ORIENTED_EDGE('',*,*,#7232,.F.);
#10074=ORIENTED_EDGE('',*,*,#7266,.T.);
#10075=ORIENTED_EDGE('',*,*,#7247,.T.);
#10076=ORIENTED_EDGE('',*,*,#7268,.F.);
#10077=ORIENTED_EDGE('',*,*,#7233,.F.);
#10078=ORIENTED_EDGE('',*,*,#7267,.T.);
#10079=ORIENTED_EDGE('',*,*,#7246,.T.);
#10080=ORIENTED_EDGE('',*,*,#7269,.T.);
#10081=ORIENTED_EDGE('',*,*,#7270,.F.);
#10082=ORIENTED_EDGE('',*,*,#7271,.F.);
#10083=ORIENTED_EDGE('',*,*,#7272,.F.);
#10084=ORIENTED_EDGE('',*,*,#7273,.T.);
#10085=ORIENTED_EDGE('',*,*,#7234,.F.);
#10086=ORIENTED_EDGE('',*,*,#7268,.T.);
#10087=ORIENTED_EDGE('',*,*,#7255,.F.);
#10088=ORIENTED_EDGE('',*,*,#7225,.F.);
#10089=ORIENTED_EDGE('',*,*,#7243,.T.);
#10090=ORIENTED_EDGE('',*,*,#7274,.T.);
#10091=ORIENTED_EDGE('',*,*,#7256,.F.);
#10092=ORIENTED_EDGE('',*,*,#7274,.F.);
#10093=ORIENTED_EDGE('',*,*,#7242,.T.);
#10094=ORIENTED_EDGE('',*,*,#7275,.T.);
#10095=ORIENTED_EDGE('',*,*,#7257,.F.);
#10096=ORIENTED_EDGE('',*,*,#7275,.F.);
#10097=ORIENTED_EDGE('',*,*,#7241,.T.);
#10098=ORIENTED_EDGE('',*,*,#7276,.T.);
#10099=ORIENTED_EDGE('',*,*,#7258,.F.);
#10100=ORIENTED_EDGE('',*,*,#7276,.F.);
#10101=ORIENTED_EDGE('',*,*,#7240,.T.);
#10102=ORIENTED_EDGE('',*,*,#7277,.T.);
#10103=ORIENTED_EDGE('',*,*,#7259,.F.);
#10104=ORIENTED_EDGE('',*,*,#7277,.F.);
#10105=ORIENTED_EDGE('',*,*,#7239,.T.);
#10106=ORIENTED_EDGE('',*,*,#7278,.T.);
#10107=ORIENTED_EDGE('',*,*,#7260,.F.);
#10108=ORIENTED_EDGE('',*,*,#7278,.F.);
#10109=ORIENTED_EDGE('',*,*,#7238,.T.);
#10110=ORIENTED_EDGE('',*,*,#7279,.T.);
#10111=ORIENTED_EDGE('',*,*,#7261,.F.);
#10112=ORIENTED_EDGE('',*,*,#7279,.F.);
#10113=ORIENTED_EDGE('',*,*,#7237,.T.);
#10114=ORIENTED_EDGE('',*,*,#7280,.T.);
#10115=ORIENTED_EDGE('',*,*,#7281,.F.);
#10116=ORIENTED_EDGE('',*,*,#7282,.T.);
#10117=ORIENTED_EDGE('',*,*,#7244,.F.);
#10118=ORIENTED_EDGE('',*,*,#7280,.F.);
#10119=ORIENTED_EDGE('',*,*,#7236,.T.);
#10120=ORIENTED_EDGE('',*,*,#7283,.T.);
#10121=ORIENTED_EDGE('',*,*,#7284,.F.);
#10122=ORIENTED_EDGE('',*,*,#7285,.F.);
#10123=ORIENTED_EDGE('',*,*,#7284,.T.);
#10124=ORIENTED_EDGE('',*,*,#7286,.T.);
#10125=ORIENTED_EDGE('',*,*,#7272,.T.);
#10126=ORIENTED_EDGE('',*,*,#7287,.F.);
#10127=ORIENTED_EDGE('',*,*,#7285,.T.);
#10128=ORIENTED_EDGE('',*,*,#7287,.T.);
#10129=ORIENTED_EDGE('',*,*,#7271,.T.);
#10130=ORIENTED_EDGE('',*,*,#7288,.F.);
#10131=ORIENTED_EDGE('',*,*,#7270,.T.);
#10132=ORIENTED_EDGE('',*,*,#7289,.T.);
#10133=ORIENTED_EDGE('',*,*,#7281,.T.);
#10134=ORIENTED_EDGE('',*,*,#7288,.T.);
#10135=ORIENTED_EDGE('',*,*,#7216,.T.);
#10136=ORIENTED_EDGE('',*,*,#7290,.T.);
#10137=ORIENTED_EDGE('',*,*,#7222,.T.);
#10138=ORIENTED_EDGE('',*,*,#7291,.T.);
#10139=ORIENTED_EDGE('',*,*,#7221,.T.);
#10140=ORIENTED_EDGE('',*,*,#7292,.T.);
#10141=ORIENTED_EDGE('',*,*,#7217,.T.);
#10142=ORIENTED_EDGE('',*,*,#7291,.F.);
#10143=ORIENTED_EDGE('',*,*,#7220,.T.);
#10144=ORIENTED_EDGE('',*,*,#7293,.T.);
#10145=ORIENTED_EDGE('',*,*,#7210,.T.);
#10146=ORIENTED_EDGE('',*,*,#7292,.F.);
#10147=ORIENTED_EDGE('',*,*,#7282,.F.);
#10148=ORIENTED_EDGE('',*,*,#7289,.F.);
#10149=ORIENTED_EDGE('',*,*,#7269,.F.);
#10150=ORIENTED_EDGE('',*,*,#7245,.F.);
#10151=ORIENTED_EDGE('',*,*,#7219,.F.);
#10152=ORIENTED_EDGE('',*,*,#7254,.F.);
#10153=ORIENTED_EDGE('',*,*,#7211,.F.);
#10154=ORIENTED_EDGE('',*,*,#7293,.F.);
#10155=ORIENTED_EDGE('',*,*,#7223,.F.);
#10156=ORIENTED_EDGE('',*,*,#7290,.F.);
#10157=ORIENTED_EDGE('',*,*,#7215,.F.);
#10158=ORIENTED_EDGE('',*,*,#7226,.F.);
#10159=ORIENTED_EDGE('',*,*,#7283,.F.);
#10160=ORIENTED_EDGE('',*,*,#7235,.F.);
#10161=ORIENTED_EDGE('',*,*,#7273,.F.);
#10162=ORIENTED_EDGE('',*,*,#7286,.F.);
#10163=ORIENTED_EDGE('',*,*,#7294,.F.);
#10164=ORIENTED_EDGE('',*,*,#7295,.T.);
#10165=ORIENTED_EDGE('',*,*,#7296,.F.);
#10166=ORIENTED_EDGE('',*,*,#7297,.F.);
#10167=ORIENTED_EDGE('',*,*,#7298,.F.);
#10168=ORIENTED_EDGE('',*,*,#7299,.T.);
#10169=ORIENTED_EDGE('',*,*,#7300,.F.);
#10170=ORIENTED_EDGE('',*,*,#7301,.F.);
#10171=ORIENTED_EDGE('',*,*,#7302,.T.);
#10172=ORIENTED_EDGE('',*,*,#7303,.T.);
#10173=ORIENTED_EDGE('',*,*,#7298,.T.);
#10174=ORIENTED_EDGE('',*,*,#7304,.T.);
#10175=ORIENTED_EDGE('',*,*,#7303,.F.);
#10176=ORIENTED_EDGE('',*,*,#7294,.T.);
#10177=ORIENTED_EDGE('',*,*,#7305,.F.);
#10178=ORIENTED_EDGE('',*,*,#7306,.T.);
#10179=ORIENTED_EDGE('',*,*,#7307,.T.);
#10180=ORIENTED_EDGE('',*,*,#7306,.F.);
#10181=ORIENTED_EDGE('',*,*,#7308,.F.);
#10182=ORIENTED_EDGE('',*,*,#7309,.F.);
#10183=ORIENTED_EDGE('',*,*,#7310,.T.);
#10184=ORIENTED_EDGE('',*,*,#7311,.T.);
#10185=ORIENTED_EDGE('',*,*,#7305,.T.);
#10186=ORIENTED_EDGE('',*,*,#7300,.T.);
#10187=ORIENTED_EDGE('',*,*,#7312,.T.);
#10188=ORIENTED_EDGE('',*,*,#7308,.T.);
#10189=ORIENTED_EDGE('',*,*,#7296,.T.);
#10190=ORIENTED_EDGE('',*,*,#7310,.F.);
#10191=ORIENTED_EDGE('',*,*,#7313,.F.);
#10192=ORIENTED_EDGE('',*,*,#7314,.T.);
#10193=ORIENTED_EDGE('',*,*,#7309,.T.);
#10194=ORIENTED_EDGE('',*,*,#7314,.F.);
#10195=ORIENTED_EDGE('',*,*,#7315,.F.);
#10196=ORIENTED_EDGE('',*,*,#7316,.F.);
#10197=ORIENTED_EDGE('',*,*,#7317,.T.);
#10198=ORIENTED_EDGE('',*,*,#7318,.T.);
#10199=ORIENTED_EDGE('',*,*,#7317,.F.);
#10200=ORIENTED_EDGE('',*,*,#7315,.T.);
#10201=ORIENTED_EDGE('',*,*,#7316,.T.);
#10202=ORIENTED_EDGE('',*,*,#7319,.T.);
#10203=ORIENTED_EDGE('',*,*,#7320,.F.);
#10204=ORIENTED_EDGE('',*,*,#7319,.F.);
#10205=ORIENTED_EDGE('',*,*,#7320,.T.);
#10206=ORIENTED_EDGE('',*,*,#7318,.F.);
#10207=ORIENTED_EDGE('',*,*,#7313,.T.);
#10208=ORIENTED_EDGE('',*,*,#7307,.F.);
#10209=ORIENTED_EDGE('',*,*,#7299,.F.);
#10210=ORIENTED_EDGE('',*,*,#7304,.F.);
#10211=ORIENTED_EDGE('',*,*,#7301,.T.);
#10212=ORIENTED_EDGE('',*,*,#7312,.F.);
#10213=ORIENTED_EDGE('',*,*,#7295,.F.);
#10214=ORIENTED_EDGE('',*,*,#7302,.F.);
#10215=ORIENTED_EDGE('',*,*,#7297,.T.);
#10216=ORIENTED_EDGE('',*,*,#7311,.F.);
#10217=ORIENTED_EDGE('',*,*,#7321,.F.);
#10218=ORIENTED_EDGE('',*,*,#7322,.T.);
#10219=ORIENTED_EDGE('',*,*,#7323,.F.);
#10220=ORIENTED_EDGE('',*,*,#7324,.F.);
#10221=ORIENTED_EDGE('',*,*,#7325,.F.);
#10222=ORIENTED_EDGE('',*,*,#7326,.T.);
#10223=ORIENTED_EDGE('',*,*,#7327,.F.);
#10224=ORIENTED_EDGE('',*,*,#7328,.F.);
#10225=ORIENTED_EDGE('',*,*,#7329,.T.);
#10226=ORIENTED_EDGE('',*,*,#7330,.T.);
#10227=ORIENTED_EDGE('',*,*,#7325,.T.);
#10228=ORIENTED_EDGE('',*,*,#7331,.T.);
#10229=ORIENTED_EDGE('',*,*,#7330,.F.);
#10230=ORIENTED_EDGE('',*,*,#7321,.T.);
#10231=ORIENTED_EDGE('',*,*,#7332,.F.);
#10232=ORIENTED_EDGE('',*,*,#7333,.T.);
#10233=ORIENTED_EDGE('',*,*,#7334,.T.);
#10234=ORIENTED_EDGE('',*,*,#7333,.F.);
#10235=ORIENTED_EDGE('',*,*,#7335,.F.);
#10236=ORIENTED_EDGE('',*,*,#7336,.F.);
#10237=ORIENTED_EDGE('',*,*,#7337,.T.);
#10238=ORIENTED_EDGE('',*,*,#7338,.T.);
#10239=ORIENTED_EDGE('',*,*,#7332,.T.);
#10240=ORIENTED_EDGE('',*,*,#7327,.T.);
#10241=ORIENTED_EDGE('',*,*,#7339,.T.);
#10242=ORIENTED_EDGE('',*,*,#7335,.T.);
#10243=ORIENTED_EDGE('',*,*,#7323,.T.);
#10244=ORIENTED_EDGE('',*,*,#7337,.F.);
#10245=ORIENTED_EDGE('',*,*,#7340,.F.);
#10246=ORIENTED_EDGE('',*,*,#7341,.T.);
#10247=ORIENTED_EDGE('',*,*,#7336,.T.);
#10248=ORIENTED_EDGE('',*,*,#7341,.F.);
#10249=ORIENTED_EDGE('',*,*,#7342,.F.);
#10250=ORIENTED_EDGE('',*,*,#7343,.F.);
#10251=ORIENTED_EDGE('',*,*,#7344,.T.);
#10252=ORIENTED_EDGE('',*,*,#7345,.T.);
#10253=ORIENTED_EDGE('',*,*,#7344,.F.);
#10254=ORIENTED_EDGE('',*,*,#7342,.T.);
#10255=ORIENTED_EDGE('',*,*,#7343,.T.);
#10256=ORIENTED_EDGE('',*,*,#7346,.T.);
#10257=ORIENTED_EDGE('',*,*,#7347,.F.);
#10258=ORIENTED_EDGE('',*,*,#7346,.F.);
#10259=ORIENTED_EDGE('',*,*,#7347,.T.);
#10260=ORIENTED_EDGE('',*,*,#7345,.F.);
#10261=ORIENTED_EDGE('',*,*,#7340,.T.);
#10262=ORIENTED_EDGE('',*,*,#7334,.F.);
#10263=ORIENTED_EDGE('',*,*,#7326,.F.);
#10264=ORIENTED_EDGE('',*,*,#7331,.F.);
#10265=ORIENTED_EDGE('',*,*,#7328,.T.);
#10266=ORIENTED_EDGE('',*,*,#7339,.F.);
#10267=ORIENTED_EDGE('',*,*,#7322,.F.);
#10268=ORIENTED_EDGE('',*,*,#7329,.F.);
#10269=ORIENTED_EDGE('',*,*,#7324,.T.);
#10270=ORIENTED_EDGE('',*,*,#7338,.F.);
#10271=ORIENTED_EDGE('',*,*,#7348,.T.);
#10272=ORIENTED_EDGE('',*,*,#7349,.T.);
#10273=ORIENTED_EDGE('',*,*,#7350,.F.);
#10274=ORIENTED_EDGE('',*,*,#7349,.F.);
#10275=ORIENTED_EDGE('',*,*,#7351,.T.);
#10276=ORIENTED_EDGE('',*,*,#7352,.T.);
#10277=ORIENTED_EDGE('',*,*,#7353,.F.);
#10278=ORIENTED_EDGE('',*,*,#7352,.F.);
#10279=ORIENTED_EDGE('',*,*,#7354,.F.);
#10280=ORIENTED_EDGE('',*,*,#7355,.F.);
#10281=ORIENTED_EDGE('',*,*,#7356,.T.);
#10282=ORIENTED_EDGE('',*,*,#7356,.F.);
#10283=ORIENTED_EDGE('',*,*,#7357,.F.);
#10284=ORIENTED_EDGE('',*,*,#7358,.F.);
#10285=ORIENTED_EDGE('',*,*,#7359,.F.);
#10286=ORIENTED_EDGE('',*,*,#7359,.T.);
#10287=ORIENTED_EDGE('',*,*,#7354,.T.);
#10288=ORIENTED_EDGE('',*,*,#7355,.T.);
#10289=ORIENTED_EDGE('',*,*,#7360,.T.);
#10290=ORIENTED_EDGE('',*,*,#7361,.F.);
#10291=ORIENTED_EDGE('',*,*,#7362,.F.);
#10292=ORIENTED_EDGE('',*,*,#7360,.F.);
#10293=ORIENTED_EDGE('',*,*,#7363,.T.);
#10294=ORIENTED_EDGE('',*,*,#7364,.T.);
#10295=ORIENTED_EDGE('',*,*,#7348,.F.);
#10296=ORIENTED_EDGE('',*,*,#7364,.F.);
#10297=ORIENTED_EDGE('',*,*,#7365,.T.);
#10298=ORIENTED_EDGE('',*,*,#7350,.T.);
#10299=ORIENTED_EDGE('',*,*,#7366,.T.);
#10300=ORIENTED_EDGE('',*,*,#7367,.F.);
#10301=ORIENTED_EDGE('',*,*,#7368,.F.);
#10302=ORIENTED_EDGE('',*,*,#7366,.F.);
#10303=ORIENTED_EDGE('',*,*,#7369,.T.);
#10304=ORIENTED_EDGE('',*,*,#7370,.T.);
#10305=ORIENTED_EDGE('',*,*,#7351,.F.);
#10306=ORIENTED_EDGE('',*,*,#7370,.F.);
#10307=ORIENTED_EDGE('',*,*,#7371,.T.);
#10308=ORIENTED_EDGE('',*,*,#7353,.T.);
#10309=ORIENTED_EDGE('',*,*,#7372,.T.);
#10310=ORIENTED_EDGE('',*,*,#7357,.T.);
#10311=ORIENTED_EDGE('',*,*,#7358,.T.);
#10312=ORIENTED_EDGE('',*,*,#7372,.F.);
#10313=ORIENTED_EDGE('',*,*,#7361,.T.);
#10314=ORIENTED_EDGE('',*,*,#7362,.T.);
#10315=ORIENTED_EDGE('',*,*,#7365,.F.);
#10316=ORIENTED_EDGE('',*,*,#7363,.F.);
#10317=ORIENTED_EDGE('',*,*,#7367,.T.);
#10318=ORIENTED_EDGE('',*,*,#7368,.T.);
#10319=ORIENTED_EDGE('',*,*,#7371,.F.);
#10320=ORIENTED_EDGE('',*,*,#7369,.F.);
#10321=ORIENTED_EDGE('',*,*,#7373,.T.);
#10322=ORIENTED_EDGE('',*,*,#7374,.T.);
#10323=ORIENTED_EDGE('',*,*,#7375,.F.);
#10324=ORIENTED_EDGE('',*,*,#7374,.F.);
#10325=ORIENTED_EDGE('',*,*,#7376,.T.);
#10326=ORIENTED_EDGE('',*,*,#7377,.T.);
#10327=ORIENTED_EDGE('',*,*,#7378,.F.);
#10328=ORIENTED_EDGE('',*,*,#7377,.F.);
#10329=ORIENTED_EDGE('',*,*,#7379,.F.);
#10330=ORIENTED_EDGE('',*,*,#7380,.F.);
#10331=ORIENTED_EDGE('',*,*,#7381,.F.);
#10332=ORIENTED_EDGE('',*,*,#7381,.T.);
#10333=ORIENTED_EDGE('',*,*,#7382,.F.);
#10334=ORIENTED_EDGE('',*,*,#7383,.F.);
#10335=ORIENTED_EDGE('',*,*,#7383,.T.);
#10336=ORIENTED_EDGE('',*,*,#7384,.F.);
#10337=ORIENTED_EDGE('',*,*,#7379,.T.);
#10338=ORIENTED_EDGE('',*,*,#7380,.T.);
#10339=ORIENTED_EDGE('',*,*,#7385,.T.);
#10340=ORIENTED_EDGE('',*,*,#7386,.F.);
#10341=ORIENTED_EDGE('',*,*,#7387,.F.);
#10342=ORIENTED_EDGE('',*,*,#7385,.F.);
#10343=ORIENTED_EDGE('',*,*,#7388,.T.);
#10344=ORIENTED_EDGE('',*,*,#7389,.T.);
#10345=ORIENTED_EDGE('',*,*,#7373,.F.);
#10346=ORIENTED_EDGE('',*,*,#7389,.F.);
#10347=ORIENTED_EDGE('',*,*,#7390,.T.);
#10348=ORIENTED_EDGE('',*,*,#7375,.T.);
#10349=ORIENTED_EDGE('',*,*,#7391,.T.);
#10350=ORIENTED_EDGE('',*,*,#7392,.F.);
#10351=ORIENTED_EDGE('',*,*,#7393,.F.);
#10352=ORIENTED_EDGE('',*,*,#7391,.F.);
#10353=ORIENTED_EDGE('',*,*,#7394,.T.);
#10354=ORIENTED_EDGE('',*,*,#7395,.T.);
#10355=ORIENTED_EDGE('',*,*,#7376,.F.);
#10356=ORIENTED_EDGE('',*,*,#7395,.F.);
#10357=ORIENTED_EDGE('',*,*,#7396,.T.);
#10358=ORIENTED_EDGE('',*,*,#7378,.T.);
#10359=ORIENTED_EDGE('',*,*,#7397,.T.);
#10360=ORIENTED_EDGE('',*,*,#7384,.T.);
#10361=ORIENTED_EDGE('',*,*,#7382,.T.);
#10362=ORIENTED_EDGE('',*,*,#7397,.F.);
#10363=ORIENTED_EDGE('',*,*,#7386,.T.);
#10364=ORIENTED_EDGE('',*,*,#7387,.T.);
#10365=ORIENTED_EDGE('',*,*,#7390,.F.);
#10366=ORIENTED_EDGE('',*,*,#7388,.F.);
#10367=ORIENTED_EDGE('',*,*,#7392,.T.);
#10368=ORIENTED_EDGE('',*,*,#7393,.T.);
#10369=ORIENTED_EDGE('',*,*,#7396,.F.);
#10370=ORIENTED_EDGE('',*,*,#7394,.F.);
#10371=ORIENTED_EDGE('',*,*,#7398,.F.);
#10372=ORIENTED_EDGE('',*,*,#7399,.T.);
#10373=ORIENTED_EDGE('',*,*,#7400,.T.);
#10374=ORIENTED_EDGE('',*,*,#7399,.F.);
#10375=ORIENTED_EDGE('',*,*,#7401,.F.);
#10376=ORIENTED_EDGE('',*,*,#7402,.T.);
#10377=ORIENTED_EDGE('',*,*,#7403,.T.);
#10378=ORIENTED_EDGE('',*,*,#7402,.F.);
#10379=ORIENTED_EDGE('',*,*,#7404,.T.);
#10380=ORIENTED_EDGE('',*,*,#7405,.T.);
#10381=ORIENTED_EDGE('',*,*,#7406,.F.);
#10382=ORIENTED_EDGE('',*,*,#7405,.F.);
#10383=ORIENTED_EDGE('',*,*,#7407,.T.);
#10384=ORIENTED_EDGE('',*,*,#7408,.T.);
#10385=ORIENTED_EDGE('',*,*,#7409,.F.);
#10386=ORIENTED_EDGE('',*,*,#7408,.F.);
#10387=ORIENTED_EDGE('',*,*,#7410,.T.);
#10388=ORIENTED_EDGE('',*,*,#7411,.T.);
#10389=ORIENTED_EDGE('',*,*,#7412,.T.);
#10390=ORIENTED_EDGE('',*,*,#7413,.F.);
#10391=ORIENTED_EDGE('',*,*,#7414,.F.);
#10392=ORIENTED_EDGE('',*,*,#7415,.T.);
#10393=ORIENTED_EDGE('',*,*,#7416,.F.);
#10394=ORIENTED_EDGE('',*,*,#7417,.F.);
#10395=ORIENTED_EDGE('',*,*,#7418,.F.);
#10396=ORIENTED_EDGE('',*,*,#7419,.F.);
#10397=ORIENTED_EDGE('',*,*,#7420,.T.);
#10398=ORIENTED_EDGE('',*,*,#7411,.F.);
#10399=ORIENTED_EDGE('',*,*,#7421,.T.);
#10400=ORIENTED_EDGE('',*,*,#7422,.T.);
#10401=ORIENTED_EDGE('',*,*,#7423,.F.);
#10402=ORIENTED_EDGE('',*,*,#7424,.F.);
#10403=ORIENTED_EDGE('',*,*,#7425,.T.);
#10404=ORIENTED_EDGE('',*,*,#7426,.T.);
#10405=ORIENTED_EDGE('',*,*,#7427,.F.);
#10406=ORIENTED_EDGE('',*,*,#7428,.T.);
#10407=ORIENTED_EDGE('',*,*,#7429,.F.);
#10408=ORIENTED_EDGE('',*,*,#7428,.F.);
#10409=ORIENTED_EDGE('',*,*,#7430,.F.);
#10410=ORIENTED_EDGE('',*,*,#7431,.F.);
#10411=ORIENTED_EDGE('',*,*,#7432,.T.);
#10412=ORIENTED_EDGE('',*,*,#7433,.F.);
#10413=ORIENTED_EDGE('',*,*,#7434,.T.);
#10414=ORIENTED_EDGE('',*,*,#7435,.T.);
#10415=ORIENTED_EDGE('',*,*,#7436,.F.);
#10416=ORIENTED_EDGE('',*,*,#7437,.F.);
#10417=ORIENTED_EDGE('',*,*,#7438,.T.);
#10418=ORIENTED_EDGE('',*,*,#7439,.T.);
#10419=ORIENTED_EDGE('',*,*,#7440,.F.);
#10420=ORIENTED_EDGE('',*,*,#7441,.T.);
#10421=ORIENTED_EDGE('',*,*,#7442,.F.);
#10422=ORIENTED_EDGE('',*,*,#7443,.F.);
#10423=ORIENTED_EDGE('',*,*,#7430,.T.);
#10424=ORIENTED_EDGE('',*,*,#7427,.T.);
#10425=ORIENTED_EDGE('',*,*,#7444,.F.);
#10426=ORIENTED_EDGE('',*,*,#7412,.F.);
#10427=ORIENTED_EDGE('',*,*,#7420,.F.);
#10428=ORIENTED_EDGE('',*,*,#7445,.T.);
#10429=ORIENTED_EDGE('',*,*,#7429,.T.);
#10430=ORIENTED_EDGE('',*,*,#7410,.F.);
#10431=ORIENTED_EDGE('',*,*,#7446,.F.);
#10432=ORIENTED_EDGE('',*,*,#7431,.T.);
#10433=ORIENTED_EDGE('',*,*,#7447,.T.);
#10434=ORIENTED_EDGE('',*,*,#7448,.F.);
#10435=ORIENTED_EDGE('',*,*,#7449,.T.);
#10436=ORIENTED_EDGE('',*,*,#7450,.F.);
#10437=ORIENTED_EDGE('',*,*,#7451,.F.);
#10438=ORIENTED_EDGE('',*,*,#7448,.T.);
#10439=ORIENTED_EDGE('',*,*,#7452,.T.);
#10440=ORIENTED_EDGE('',*,*,#7453,.F.);
#10441=ORIENTED_EDGE('',*,*,#7454,.F.);
#10442=ORIENTED_EDGE('',*,*,#7450,.T.);
#10443=ORIENTED_EDGE('',*,*,#7455,.F.);
#10444=ORIENTED_EDGE('',*,*,#7439,.F.);
#10445=ORIENTED_EDGE('',*,*,#7456,.T.);
#10446=ORIENTED_EDGE('',*,*,#7453,.T.);
#10447=ORIENTED_EDGE('',*,*,#7451,.T.);
#10448=ORIENTED_EDGE('',*,*,#7454,.T.);
#10449=ORIENTED_EDGE('',*,*,#7456,.F.);
#10450=ORIENTED_EDGE('',*,*,#7438,.F.);
#10451=ORIENTED_EDGE('',*,*,#7432,.F.);
#10452=ORIENTED_EDGE('',*,*,#7446,.T.);
#10453=ORIENTED_EDGE('',*,*,#7404,.F.);
#10454=ORIENTED_EDGE('',*,*,#7407,.F.);
#10455=ORIENTED_EDGE('',*,*,#7449,.F.);
#10456=ORIENTED_EDGE('',*,*,#7447,.F.);
#10457=ORIENTED_EDGE('',*,*,#7445,.F.);
#10458=ORIENTED_EDGE('',*,*,#7419,.T.);
#10459=ORIENTED_EDGE('',*,*,#7436,.T.);
#10460=ORIENTED_EDGE('',*,*,#7455,.T.);
#10461=ORIENTED_EDGE('',*,*,#7452,.F.);
#10462=ORIENTED_EDGE('',*,*,#7406,.T.);
#10463=ORIENTED_EDGE('',*,*,#7409,.T.);
#10464=ORIENTED_EDGE('',*,*,#7426,.F.);
#10465=ORIENTED_EDGE('',*,*,#7457,.T.);
#10466=ORIENTED_EDGE('',*,*,#7458,.T.);
#10467=ORIENTED_EDGE('',*,*,#7459,.F.);
#10468=ORIENTED_EDGE('',*,*,#7460,.F.);
#10469=ORIENTED_EDGE('',*,*,#7458,.F.);
#10470=ORIENTED_EDGE('',*,*,#7461,.T.);
#10471=ORIENTED_EDGE('',*,*,#7462,.T.);
#10472=ORIENTED_EDGE('',*,*,#7463,.T.);
#10473=ORIENTED_EDGE('',*,*,#7464,.F.);
#10474=ORIENTED_EDGE('',*,*,#7465,.F.);
#10475=ORIENTED_EDGE('',*,*,#7442,.T.);
#10476=ORIENTED_EDGE('',*,*,#7466,.F.);
#10477=ORIENTED_EDGE('',*,*,#7462,.F.);
#10478=ORIENTED_EDGE('',*,*,#7467,.T.);
#10479=ORIENTED_EDGE('',*,*,#7464,.T.);
#10480=ORIENTED_EDGE('',*,*,#7461,.F.);
#10481=ORIENTED_EDGE('',*,*,#7457,.F.);
#10482=ORIENTED_EDGE('',*,*,#7425,.F.);
#10483=ORIENTED_EDGE('',*,*,#7443,.T.);
#10484=ORIENTED_EDGE('',*,*,#7465,.T.);
#10485=ORIENTED_EDGE('',*,*,#7467,.F.);
#10486=ORIENTED_EDGE('',*,*,#7398,.T.);
#10487=ORIENTED_EDGE('',*,*,#7401,.T.);
#10488=ORIENTED_EDGE('',*,*,#7460,.T.);
#10489=ORIENTED_EDGE('',*,*,#7466,.T.);
#10490=ORIENTED_EDGE('',*,*,#7463,.F.);
#10491=ORIENTED_EDGE('',*,*,#7441,.F.);
#10492=ORIENTED_EDGE('',*,*,#7413,.T.);
#10493=ORIENTED_EDGE('',*,*,#7444,.T.);
#10494=ORIENTED_EDGE('',*,*,#7459,.T.);
#10495=ORIENTED_EDGE('',*,*,#7400,.F.);
#10496=ORIENTED_EDGE('',*,*,#7403,.F.);
#10497=ORIENTED_EDGE('',*,*,#7468,.T.);
#10498=ORIENTED_EDGE('',*,*,#7415,.F.);
#10499=ORIENTED_EDGE('',*,*,#7469,.F.);
#10500=ORIENTED_EDGE('',*,*,#7417,.T.);
#10501=ORIENTED_EDGE('',*,*,#7423,.T.);
#10502=ORIENTED_EDGE('',*,*,#7470,.T.);
#10503=ORIENTED_EDGE('',*,*,#7434,.F.);
#10504=ORIENTED_EDGE('',*,*,#7471,.F.);
#10505=ORIENTED_EDGE('',*,*,#7418,.T.);
#10506=ORIENTED_EDGE('',*,*,#7469,.T.);
#10507=ORIENTED_EDGE('',*,*,#7414,.T.);
#10508=ORIENTED_EDGE('',*,*,#7440,.T.);
#10509=ORIENTED_EDGE('',*,*,#7424,.T.);
#10510=ORIENTED_EDGE('',*,*,#7471,.T.);
#10511=ORIENTED_EDGE('',*,*,#7433,.T.);
#10512=ORIENTED_EDGE('',*,*,#7437,.T.);
#10513=ORIENTED_EDGE('',*,*,#7468,.F.);
#10514=ORIENTED_EDGE('',*,*,#7416,.T.);
#10515=ORIENTED_EDGE('',*,*,#7421,.F.);
#10516=ORIENTED_EDGE('',*,*,#7472,.T.);
#10517=ORIENTED_EDGE('',*,*,#7422,.F.);
#10518=ORIENTED_EDGE('',*,*,#7472,.F.);
#10519=ORIENTED_EDGE('',*,*,#7435,.F.);
#10520=ORIENTED_EDGE('',*,*,#7470,.F.);
#10521=ORIENTED_EDGE('',*,*,#7473,.F.);
#10522=ORIENTED_EDGE('',*,*,#7474,.F.);
#10523=ORIENTED_EDGE('',*,*,#7475,.T.);
#10524=ORIENTED_EDGE('',*,*,#7476,.F.);
#10525=ORIENTED_EDGE('',*,*,#7477,.F.);
#10526=ORIENTED_EDGE('',*,*,#7475,.F.);
#10527=ORIENTED_EDGE('',*,*,#7473,.T.);
#10528=ORIENTED_EDGE('',*,*,#7474,.T.);
#10529=ORIENTED_EDGE('',*,*,#7478,.T.);
#10530=ORIENTED_EDGE('',*,*,#7479,.F.);
#10531=ORIENTED_EDGE('',*,*,#7478,.F.);
#10532=ORIENTED_EDGE('',*,*,#7480,.T.);
#10533=ORIENTED_EDGE('',*,*,#7481,.T.);
#10534=ORIENTED_EDGE('',*,*,#7476,.T.);
#10535=ORIENTED_EDGE('',*,*,#7477,.T.);
#10536=ORIENTED_EDGE('',*,*,#7481,.F.);
#10537=ORIENTED_EDGE('',*,*,#7480,.F.);
#10538=ORIENTED_EDGE('',*,*,#7479,.T.);
#10539=ORIENTED_EDGE('',*,*,#7482,.F.);
#10540=ORIENTED_EDGE('',*,*,#7483,.T.);
#10541=ORIENTED_EDGE('',*,*,#7484,.F.);
#10542=ORIENTED_EDGE('',*,*,#7485,.F.);
#10543=ORIENTED_EDGE('',*,*,#7483,.F.);
#10544=ORIENTED_EDGE('',*,*,#7486,.F.);
#10545=ORIENTED_EDGE('',*,*,#7487,.F.);
#10546=ORIENTED_EDGE('',*,*,#7488,.T.);
#10547=ORIENTED_EDGE('',*,*,#7489,.F.);
#10548=ORIENTED_EDGE('',*,*,#7488,.F.);
#10549=ORIENTED_EDGE('',*,*,#7486,.T.);
#10550=ORIENTED_EDGE('',*,*,#7487,.T.);
#10551=ORIENTED_EDGE('',*,*,#7490,.T.);
#10552=ORIENTED_EDGE('',*,*,#7484,.T.);
#10553=ORIENTED_EDGE('',*,*,#7485,.T.);
#10554=ORIENTED_EDGE('',*,*,#7490,.F.);
#10555=ORIENTED_EDGE('',*,*,#7491,.T.);
#10556=ORIENTED_EDGE('',*,*,#7492,.T.);
#10557=ORIENTED_EDGE('',*,*,#7493,.F.);
#10558=ORIENTED_EDGE('',*,*,#7492,.F.);
#10559=ORIENTED_EDGE('',*,*,#7482,.T.);
#10560=ORIENTED_EDGE('',*,*,#7489,.T.);
#10561=ORIENTED_EDGE('',*,*,#7493,.T.);
#10562=ORIENTED_EDGE('',*,*,#7491,.F.);
#10563=ORIENTED_EDGE('',*,*,#7494,.F.);
#10564=ORIENTED_EDGE('',*,*,#7495,.T.);
#10565=ORIENTED_EDGE('',*,*,#7496,.F.);
#10566=ORIENTED_EDGE('',*,*,#7495,.F.);
#10567=ORIENTED_EDGE('',*,*,#7497,.F.);
#10568=ORIENTED_EDGE('',*,*,#7498,.F.);
#10569=ORIENTED_EDGE('',*,*,#7499,.T.);
#10570=ORIENTED_EDGE('',*,*,#7500,.F.);
#10571=ORIENTED_EDGE('',*,*,#7499,.F.);
#10572=ORIENTED_EDGE('',*,*,#7497,.T.);
#10573=ORIENTED_EDGE('',*,*,#7498,.T.);
#10574=ORIENTED_EDGE('',*,*,#7501,.T.);
#10575=ORIENTED_EDGE('',*,*,#7494,.T.);
#10576=ORIENTED_EDGE('',*,*,#7501,.F.);
#10577=ORIENTED_EDGE('',*,*,#7496,.T.);
#10578=ORIENTED_EDGE('',*,*,#7500,.T.);
#10579=ORIENTED_EDGE('',*,*,#7502,.F.);
#10580=ORIENTED_EDGE('',*,*,#7503,.F.);
#10581=ORIENTED_EDGE('',*,*,#7504,.T.);
#10582=ORIENTED_EDGE('',*,*,#7505,.F.);
#10583=ORIENTED_EDGE('',*,*,#7504,.F.);
#10584=ORIENTED_EDGE('',*,*,#7506,.F.);
#10585=ORIENTED_EDGE('',*,*,#7507,.T.);
#10586=ORIENTED_EDGE('',*,*,#7508,.F.);
#10587=ORIENTED_EDGE('',*,*,#7507,.F.);
#10588=ORIENTED_EDGE('',*,*,#7509,.F.);
#10589=ORIENTED_EDGE('',*,*,#7510,.T.);
#10590=ORIENTED_EDGE('',*,*,#7511,.F.);
#10591=ORIENTED_EDGE('',*,*,#7512,.F.);
#10592=ORIENTED_EDGE('',*,*,#7510,.F.);
#10593=ORIENTED_EDGE('',*,*,#7513,.F.);
#10594=ORIENTED_EDGE('',*,*,#7514,.T.);
#10595=ORIENTED_EDGE('',*,*,#7515,.F.);
#10596=ORIENTED_EDGE('',*,*,#7514,.F.);
#10597=ORIENTED_EDGE('',*,*,#7516,.F.);
#10598=ORIENTED_EDGE('',*,*,#7517,.F.);
#10599=ORIENTED_EDGE('',*,*,#7518,.T.);
#10600=ORIENTED_EDGE('',*,*,#7519,.F.);
#10601=ORIENTED_EDGE('',*,*,#7518,.F.);
#10602=ORIENTED_EDGE('',*,*,#7520,.F.);
#10603=ORIENTED_EDGE('',*,*,#7521,.T.);
#10604=ORIENTED_EDGE('',*,*,#7522,.F.);
#10605=ORIENTED_EDGE('',*,*,#7523,.F.);
#10606=ORIENTED_EDGE('',*,*,#7521,.F.);
#10607=ORIENTED_EDGE('',*,*,#7524,.T.);
#10608=ORIENTED_EDGE('',*,*,#7525,.T.);
#10609=ORIENTED_EDGE('',*,*,#7526,.T.);
#10610=ORIENTED_EDGE('',*,*,#7525,.F.);
#10611=ORIENTED_EDGE('',*,*,#7527,.T.);
#10612=ORIENTED_EDGE('',*,*,#7528,.T.);
#10613=ORIENTED_EDGE('',*,*,#7529,.F.);
#10614=ORIENTED_EDGE('',*,*,#7528,.F.);
#10615=ORIENTED_EDGE('',*,*,#7515,.T.);
#10616=ORIENTED_EDGE('',*,*,#7530,.T.);
#10617=ORIENTED_EDGE('',*,*,#7506,.T.);
#10618=ORIENTED_EDGE('',*,*,#7530,.F.);
#10619=ORIENTED_EDGE('',*,*,#7531,.F.);
#10620=ORIENTED_EDGE('',*,*,#7532,.T.);
#10621=ORIENTED_EDGE('',*,*,#7533,.T.);
#10622=ORIENTED_EDGE('',*,*,#7532,.F.);
#10623=ORIENTED_EDGE('',*,*,#7502,.T.);
#10624=ORIENTED_EDGE('',*,*,#7503,.T.);
#10625=ORIENTED_EDGE('',*,*,#7534,.T.);
#10626=ORIENTED_EDGE('',*,*,#7522,.T.);
#10627=ORIENTED_EDGE('',*,*,#7523,.T.);
#10628=ORIENTED_EDGE('',*,*,#7534,.F.);
#10629=ORIENTED_EDGE('',*,*,#7516,.T.);
#10630=ORIENTED_EDGE('',*,*,#7517,.T.);
#10631=ORIENTED_EDGE('',*,*,#7535,.T.);
#10632=ORIENTED_EDGE('',*,*,#7511,.T.);
#10633=ORIENTED_EDGE('',*,*,#7512,.T.);
#10634=ORIENTED_EDGE('',*,*,#7535,.F.);
#10635=ORIENTED_EDGE('',*,*,#7509,.T.);
#10636=ORIENTED_EDGE('',*,*,#7508,.T.);
#10637=ORIENTED_EDGE('',*,*,#7519,.T.);
#10638=ORIENTED_EDGE('',*,*,#7505,.T.);
#10639=ORIENTED_EDGE('',*,*,#7520,.T.);
#10640=ORIENTED_EDGE('',*,*,#7531,.T.);
#10641=ORIENTED_EDGE('',*,*,#7513,.T.);
#10642=ORIENTED_EDGE('',*,*,#7527,.F.);
#10643=ORIENTED_EDGE('',*,*,#7533,.F.);
#10644=ORIENTED_EDGE('',*,*,#7524,.F.);
#10645=ORIENTED_EDGE('',*,*,#7529,.T.);
#10646=ORIENTED_EDGE('',*,*,#7526,.F.);
#10647=ORIENTED_EDGE('',*,*,#7536,.F.);
#10648=ORIENTED_EDGE('',*,*,#7537,.F.);
#10649=ORIENTED_EDGE('',*,*,#7538,.T.);
#10650=ORIENTED_EDGE('',*,*,#7539,.F.);
#10651=ORIENTED_EDGE('',*,*,#7538,.F.);
#10652=ORIENTED_EDGE('',*,*,#7540,.F.);
#10653=ORIENTED_EDGE('',*,*,#7541,.T.);
#10654=ORIENTED_EDGE('',*,*,#7542,.F.);
#10655=ORIENTED_EDGE('',*,*,#7541,.F.);
#10656=ORIENTED_EDGE('',*,*,#7543,.F.);
#10657=ORIENTED_EDGE('',*,*,#7544,.T.);
#10658=ORIENTED_EDGE('',*,*,#7545,.F.);
#10659=ORIENTED_EDGE('',*,*,#7546,.F.);
#10660=ORIENTED_EDGE('',*,*,#7544,.F.);
#10661=ORIENTED_EDGE('',*,*,#7547,.F.);
#10662=ORIENTED_EDGE('',*,*,#7548,.T.);
#10663=ORIENTED_EDGE('',*,*,#7549,.F.);
#10664=ORIENTED_EDGE('',*,*,#7548,.F.);
#10665=ORIENTED_EDGE('',*,*,#7550,.F.);
#10666=ORIENTED_EDGE('',*,*,#7551,.F.);
#10667=ORIENTED_EDGE('',*,*,#7552,.T.);
#10668=ORIENTED_EDGE('',*,*,#7553,.F.);
#10669=ORIENTED_EDGE('',*,*,#7552,.F.);
#10670=ORIENTED_EDGE('',*,*,#7554,.F.);
#10671=ORIENTED_EDGE('',*,*,#7555,.T.);
#10672=ORIENTED_EDGE('',*,*,#7556,.F.);
#10673=ORIENTED_EDGE('',*,*,#7557,.F.);
#10674=ORIENTED_EDGE('',*,*,#7555,.F.);
#10675=ORIENTED_EDGE('',*,*,#7558,.T.);
#10676=ORIENTED_EDGE('',*,*,#7559,.T.);
#10677=ORIENTED_EDGE('',*,*,#7560,.T.);
#10678=ORIENTED_EDGE('',*,*,#7559,.F.);
#10679=ORIENTED_EDGE('',*,*,#7561,.T.);
#10680=ORIENTED_EDGE('',*,*,#7562,.T.);
#10681=ORIENTED_EDGE('',*,*,#7563,.F.);
#10682=ORIENTED_EDGE('',*,*,#7562,.F.);
#10683=ORIENTED_EDGE('',*,*,#7549,.T.);
#10684=ORIENTED_EDGE('',*,*,#7564,.T.);
#10685=ORIENTED_EDGE('',*,*,#7540,.T.);
#10686=ORIENTED_EDGE('',*,*,#7564,.F.);
#10687=ORIENTED_EDGE('',*,*,#7565,.F.);
#10688=ORIENTED_EDGE('',*,*,#7566,.T.);
#10689=ORIENTED_EDGE('',*,*,#7567,.T.);
#10690=ORIENTED_EDGE('',*,*,#7566,.F.);
#10691=ORIENTED_EDGE('',*,*,#7536,.T.);
#10692=ORIENTED_EDGE('',*,*,#7537,.T.);
#10693=ORIENTED_EDGE('',*,*,#7568,.T.);
#10694=ORIENTED_EDGE('',*,*,#7556,.T.);
#10695=ORIENTED_EDGE('',*,*,#7557,.T.);
#10696=ORIENTED_EDGE('',*,*,#7568,.F.);
#10697=ORIENTED_EDGE('',*,*,#7550,.T.);
#10698=ORIENTED_EDGE('',*,*,#7551,.T.);
#10699=ORIENTED_EDGE('',*,*,#7569,.T.);
#10700=ORIENTED_EDGE('',*,*,#7545,.T.);
#10701=ORIENTED_EDGE('',*,*,#7546,.T.);
#10702=ORIENTED_EDGE('',*,*,#7569,.F.);
#10703=ORIENTED_EDGE('',*,*,#7543,.T.);
#10704=ORIENTED_EDGE('',*,*,#7542,.T.);
#10705=ORIENTED_EDGE('',*,*,#7553,.T.);
#10706=ORIENTED_EDGE('',*,*,#7539,.T.);
#10707=ORIENTED_EDGE('',*,*,#7554,.T.);
#10708=ORIENTED_EDGE('',*,*,#7565,.T.);
#10709=ORIENTED_EDGE('',*,*,#7547,.T.);
#10710=ORIENTED_EDGE('',*,*,#7561,.F.);
#10711=ORIENTED_EDGE('',*,*,#7567,.F.);
#10712=ORIENTED_EDGE('',*,*,#7558,.F.);
#10713=ORIENTED_EDGE('',*,*,#7563,.T.);
#10714=ORIENTED_EDGE('',*,*,#7560,.F.);
#10715=ORIENTED_EDGE('',*,*,#7570,.F.);
#10716=ORIENTED_EDGE('',*,*,#7571,.T.);
#10717=ORIENTED_EDGE('',*,*,#7572,.F.);
#10718=ORIENTED_EDGE('',*,*,#7571,.F.);
#10719=ORIENTED_EDGE('',*,*,#7573,.F.);
#10720=ORIENTED_EDGE('',*,*,#7574,.F.);
#10721=ORIENTED_EDGE('',*,*,#7575,.T.);
#10722=ORIENTED_EDGE('',*,*,#7576,.F.);
#10723=ORIENTED_EDGE('',*,*,#7575,.F.);
#10724=ORIENTED_EDGE('',*,*,#7573,.T.);
#10725=ORIENTED_EDGE('',*,*,#7574,.T.);
#10726=ORIENTED_EDGE('',*,*,#7577,.T.);
#10727=ORIENTED_EDGE('',*,*,#7570,.T.);
#10728=ORIENTED_EDGE('',*,*,#7577,.F.);
#10729=ORIENTED_EDGE('',*,*,#7572,.T.);
#10730=ORIENTED_EDGE('',*,*,#7576,.T.);
#10731=ORIENTED_EDGE('',*,*,#7578,.F.);
#10732=ORIENTED_EDGE('',*,*,#7579,.T.);
#10733=ORIENTED_EDGE('',*,*,#7580,.T.);
#10734=ORIENTED_EDGE('',*,*,#7581,.F.);
#10735=ORIENTED_EDGE('',*,*,#7582,.F.);
#10736=ORIENTED_EDGE('',*,*,#7583,.T.);
#10737=ORIENTED_EDGE('',*,*,#7578,.T.);
#10738=ORIENTED_EDGE('',*,*,#7584,.F.);
#10739=ORIENTED_EDGE('',*,*,#7585,.F.);
#10740=ORIENTED_EDGE('',*,*,#7586,.T.);
#10741=ORIENTED_EDGE('',*,*,#7582,.T.);
#10742=ORIENTED_EDGE('',*,*,#7587,.F.);
#10743=ORIENTED_EDGE('',*,*,#7588,.F.);
#10744=ORIENTED_EDGE('',*,*,#7589,.T.);
#10745=ORIENTED_EDGE('',*,*,#7585,.T.);
#10746=ORIENTED_EDGE('',*,*,#7590,.F.);
#10747=ORIENTED_EDGE('',*,*,#7591,.F.);
#10748=ORIENTED_EDGE('',*,*,#7592,.T.);
#10749=ORIENTED_EDGE('',*,*,#7588,.T.);
#10750=ORIENTED_EDGE('',*,*,#7593,.F.);
#10751=ORIENTED_EDGE('',*,*,#7594,.F.);
#10752=ORIENTED_EDGE('',*,*,#7595,.T.);
#10753=ORIENTED_EDGE('',*,*,#7591,.T.);
#10754=ORIENTED_EDGE('',*,*,#7596,.F.);
#10755=ORIENTED_EDGE('',*,*,#7597,.F.);
#10756=ORIENTED_EDGE('',*,*,#7598,.T.);
#10757=ORIENTED_EDGE('',*,*,#7594,.T.);
#10758=ORIENTED_EDGE('',*,*,#7599,.F.);
#10759=ORIENTED_EDGE('',*,*,#7600,.F.);
#10760=ORIENTED_EDGE('',*,*,#7601,.T.);
#10761=ORIENTED_EDGE('',*,*,#7597,.T.);
#10762=ORIENTED_EDGE('',*,*,#7602,.F.);
#10763=ORIENTED_EDGE('',*,*,#7603,.F.);
#10764=ORIENTED_EDGE('',*,*,#7604,.T.);
#10765=ORIENTED_EDGE('',*,*,#7600,.T.);
#10766=ORIENTED_EDGE('',*,*,#7605,.F.);
#10767=ORIENTED_EDGE('',*,*,#7606,.F.);
#10768=ORIENTED_EDGE('',*,*,#7607,.T.);
#10769=ORIENTED_EDGE('',*,*,#7603,.T.);
#10770=ORIENTED_EDGE('',*,*,#7608,.F.);
#10771=ORIENTED_EDGE('',*,*,#7609,.F.);
#10772=ORIENTED_EDGE('',*,*,#7610,.T.);
#10773=ORIENTED_EDGE('',*,*,#7606,.T.);
#10774=ORIENTED_EDGE('',*,*,#7611,.F.);
#10775=ORIENTED_EDGE('',*,*,#7612,.F.);
#10776=ORIENTED_EDGE('',*,*,#7613,.T.);
#10777=ORIENTED_EDGE('',*,*,#7609,.T.);
#10778=ORIENTED_EDGE('',*,*,#7614,.F.);
#10779=ORIENTED_EDGE('',*,*,#7615,.F.);
#10780=ORIENTED_EDGE('',*,*,#7616,.T.);
#10781=ORIENTED_EDGE('',*,*,#7612,.T.);
#10782=ORIENTED_EDGE('',*,*,#7617,.F.);
#10783=ORIENTED_EDGE('',*,*,#7618,.F.);
#10784=ORIENTED_EDGE('',*,*,#7619,.T.);
#10785=ORIENTED_EDGE('',*,*,#7620,.T.);
#10786=ORIENTED_EDGE('',*,*,#7621,.T.);
#10787=ORIENTED_EDGE('',*,*,#7620,.F.);
#10788=ORIENTED_EDGE('',*,*,#7622,.T.);
#10789=ORIENTED_EDGE('',*,*,#7623,.T.);
#10790=ORIENTED_EDGE('',*,*,#7624,.F.);
#10791=ORIENTED_EDGE('',*,*,#7625,.F.);
#10792=ORIENTED_EDGE('',*,*,#7626,.T.);
#10793=ORIENTED_EDGE('',*,*,#7618,.T.);
#10794=ORIENTED_EDGE('',*,*,#7627,.F.);
#10795=ORIENTED_EDGE('',*,*,#7628,.F.);
#10796=ORIENTED_EDGE('',*,*,#7629,.T.);
#10797=ORIENTED_EDGE('',*,*,#7625,.T.);
#10798=ORIENTED_EDGE('',*,*,#7630,.F.);
#10799=ORIENTED_EDGE('',*,*,#7631,.F.);
#10800=ORIENTED_EDGE('',*,*,#7632,.T.);
#10801=ORIENTED_EDGE('',*,*,#7628,.T.);
#10802=ORIENTED_EDGE('',*,*,#7633,.F.);
#10803=ORIENTED_EDGE('',*,*,#7634,.F.);
#10804=ORIENTED_EDGE('',*,*,#7635,.T.);
#10805=ORIENTED_EDGE('',*,*,#7631,.T.);
#10806=ORIENTED_EDGE('',*,*,#7636,.F.);
#10807=ORIENTED_EDGE('',*,*,#7637,.F.);
#10808=ORIENTED_EDGE('',*,*,#7638,.T.);
#10809=ORIENTED_EDGE('',*,*,#7634,.T.);
#10810=ORIENTED_EDGE('',*,*,#7639,.F.);
#10811=ORIENTED_EDGE('',*,*,#7640,.F.);
#10812=ORIENTED_EDGE('',*,*,#7641,.T.);
#10813=ORIENTED_EDGE('',*,*,#7637,.T.);
#10814=ORIENTED_EDGE('',*,*,#7642,.F.);
#10815=ORIENTED_EDGE('',*,*,#7643,.F.);
#10816=ORIENTED_EDGE('',*,*,#7644,.T.);
#10817=ORIENTED_EDGE('',*,*,#7640,.T.);
#10818=ORIENTED_EDGE('',*,*,#7645,.F.);
#10819=ORIENTED_EDGE('',*,*,#7646,.F.);
#10820=ORIENTED_EDGE('',*,*,#7647,.T.);
#10821=ORIENTED_EDGE('',*,*,#7643,.T.);
#10822=ORIENTED_EDGE('',*,*,#7648,.F.);
#10823=ORIENTED_EDGE('',*,*,#7649,.F.);
#10824=ORIENTED_EDGE('',*,*,#7650,.T.);
#10825=ORIENTED_EDGE('',*,*,#7646,.T.);
#10826=ORIENTED_EDGE('',*,*,#7651,.F.);
#10827=ORIENTED_EDGE('',*,*,#7652,.F.);
#10828=ORIENTED_EDGE('',*,*,#7653,.T.);
#10829=ORIENTED_EDGE('',*,*,#7649,.T.);
#10830=ORIENTED_EDGE('',*,*,#7654,.F.);
#10831=ORIENTED_EDGE('',*,*,#7655,.F.);
#10832=ORIENTED_EDGE('',*,*,#7656,.T.);
#10833=ORIENTED_EDGE('',*,*,#7652,.T.);
#10834=ORIENTED_EDGE('',*,*,#7657,.F.);
#10835=ORIENTED_EDGE('',*,*,#7655,.T.);
#10836=ORIENTED_EDGE('',*,*,#7658,.F.);
#10837=ORIENTED_EDGE('',*,*,#7659,.T.);
#10838=ORIENTED_EDGE('',*,*,#7660,.T.);
#10839=ORIENTED_EDGE('',*,*,#7661,.F.);
#10840=ORIENTED_EDGE('',*,*,#7662,.T.);
#10841=ORIENTED_EDGE('',*,*,#7663,.T.);
#10842=ORIENTED_EDGE('',*,*,#7664,.T.);
#10843=ORIENTED_EDGE('',*,*,#7665,.T.);
#10844=ORIENTED_EDGE('',*,*,#7666,.T.);
#10845=ORIENTED_EDGE('',*,*,#7662,.F.);
#10846=ORIENTED_EDGE('',*,*,#7667,.T.);
#10847=ORIENTED_EDGE('',*,*,#7668,.T.);
#10848=ORIENTED_EDGE('',*,*,#7669,.T.);
#10849=ORIENTED_EDGE('',*,*,#7668,.F.);
#10850=ORIENTED_EDGE('',*,*,#7670,.F.);
#10851=ORIENTED_EDGE('',*,*,#7671,.T.);
#10852=ORIENTED_EDGE('',*,*,#7672,.T.);
#10853=ORIENTED_EDGE('',*,*,#7671,.F.);
#10854=ORIENTED_EDGE('',*,*,#7673,.T.);
#10855=ORIENTED_EDGE('',*,*,#7674,.T.);
#10856=ORIENTED_EDGE('',*,*,#7675,.F.);
#10857=ORIENTED_EDGE('',*,*,#7674,.F.);
#10858=ORIENTED_EDGE('',*,*,#7676,.T.);
#10859=ORIENTED_EDGE('',*,*,#7677,.T.);
#10860=ORIENTED_EDGE('',*,*,#7678,.T.);
#10861=ORIENTED_EDGE('',*,*,#7659,.F.);
#10862=ORIENTED_EDGE('',*,*,#7679,.T.);
#10863=ORIENTED_EDGE('',*,*,#7680,.T.);
#10864=ORIENTED_EDGE('',*,*,#7663,.F.);
#10865=ORIENTED_EDGE('',*,*,#7666,.F.);
#10866=ORIENTED_EDGE('',*,*,#7681,.T.);
#10867=ORIENTED_EDGE('',*,*,#7682,.F.);
#10868=ORIENTED_EDGE('',*,*,#7683,.T.);
#10869=ORIENTED_EDGE('',*,*,#7665,.F.);
#10870=ORIENTED_EDGE('',*,*,#7684,.F.);
#10871=ORIENTED_EDGE('',*,*,#7685,.T.);
#10872=ORIENTED_EDGE('',*,*,#7686,.F.);
#10873=ORIENTED_EDGE('',*,*,#7687,.F.);
#10874=ORIENTED_EDGE('',*,*,#7672,.F.);
#10875=ORIENTED_EDGE('',*,*,#7688,.T.);
#10876=ORIENTED_EDGE('',*,*,#7689,.T.);
#10877=ORIENTED_EDGE('',*,*,#7690,.T.);
#10878=ORIENTED_EDGE('',*,*,#7691,.T.);
#10879=ORIENTED_EDGE('',*,*,#7670,.T.);
#10880=ORIENTED_EDGE('',*,*,#7664,.F.);
#10881=ORIENTED_EDGE('',*,*,#7692,.T.);
#10882=ORIENTED_EDGE('',*,*,#7693,.F.);
#10883=ORIENTED_EDGE('',*,*,#7694,.F.);
#10884=ORIENTED_EDGE('',*,*,#7695,.T.);
#10885=ORIENTED_EDGE('',*,*,#7696,.F.);
#10886=ORIENTED_EDGE('',*,*,#7697,.F.);
#10887=ORIENTED_EDGE('',*,*,#7669,.F.);
#10888=ORIENTED_EDGE('',*,*,#7698,.F.);
#10889=ORIENTED_EDGE('',*,*,#7699,.T.);
#10890=ORIENTED_EDGE('',*,*,#7700,.F.);
#10891=ORIENTED_EDGE('',*,*,#7701,.F.);
#10892=ORIENTED_EDGE('',*,*,#7667,.F.);
#10893=ORIENTED_EDGE('',*,*,#7702,.T.);
#10894=ORIENTED_EDGE('',*,*,#7703,.T.);
#10895=ORIENTED_EDGE('',*,*,#7704,.F.);
#10896=ORIENTED_EDGE('',*,*,#7705,.T.);
#10897=ORIENTED_EDGE('',*,*,#7706,.F.);
#10898=ORIENTED_EDGE('',*,*,#7707,.T.);
#10899=ORIENTED_EDGE('',*,*,#7679,.F.);
#10900=ORIENTED_EDGE('',*,*,#7708,.T.);
#10901=ORIENTED_EDGE('',*,*,#7709,.F.);
#10902=ORIENTED_EDGE('',*,*,#7702,.F.);
#10903=ORIENTED_EDGE('',*,*,#7693,.T.);
#10904=ORIENTED_EDGE('',*,*,#7710,.T.);
#10905=ORIENTED_EDGE('',*,*,#7711,.T.);
#10906=ORIENTED_EDGE('',*,*,#7704,.T.);
#10907=ORIENTED_EDGE('',*,*,#7712,.T.);
#10908=ORIENTED_EDGE('',*,*,#7713,.T.);
#10909=ORIENTED_EDGE('',*,*,#7682,.T.);
#10910=ORIENTED_EDGE('',*,*,#7696,.T.);
#10911=ORIENTED_EDGE('',*,*,#7714,.T.);
#10912=ORIENTED_EDGE('',*,*,#7712,.F.);
#10913=ORIENTED_EDGE('',*,*,#7715,.T.);
#10914=ORIENTED_EDGE('',*,*,#7698,.T.);
#10915=ORIENTED_EDGE('',*,*,#7716,.T.);
#10916=ORIENTED_EDGE('',*,*,#7709,.T.);
#10917=ORIENTED_EDGE('',*,*,#7717,.T.);
#10918=ORIENTED_EDGE('',*,*,#7694,.T.);
#10919=ORIENTED_EDGE('',*,*,#7718,.F.);
#10920=ORIENTED_EDGE('',*,*,#7700,.T.);
#10921=ORIENTED_EDGE('',*,*,#7719,.T.);
#10922=ORIENTED_EDGE('',*,*,#7697,.T.);
#10923=ORIENTED_EDGE('',*,*,#7716,.F.);
#10924=ORIENTED_EDGE('',*,*,#7701,.T.);
#10925=ORIENTED_EDGE('',*,*,#7718,.T.);
#10926=ORIENTED_EDGE('',*,*,#7687,.T.);
#10927=ORIENTED_EDGE('',*,*,#7720,.F.);
#10928=ORIENTED_EDGE('',*,*,#7691,.F.);
#10929=ORIENTED_EDGE('',*,*,#7721,.T.);
#10930=ORIENTED_EDGE('',*,*,#7690,.F.);
#10931=ORIENTED_EDGE('',*,*,#7722,.T.);
#10932=ORIENTED_EDGE('',*,*,#7706,.T.);
#10933=ORIENTED_EDGE('',*,*,#7723,.T.);
#10934=ORIENTED_EDGE('',*,*,#7684,.T.);
#10935=ORIENTED_EDGE('',*,*,#7721,.F.);
#10936=ORIENTED_EDGE('',*,*,#7711,.F.);
#10937=ORIENTED_EDGE('',*,*,#7724,.T.);
#10938=ORIENTED_EDGE('',*,*,#7688,.F.);
#10939=ORIENTED_EDGE('',*,*,#7720,.T.);
#10940=ORIENTED_EDGE('',*,*,#7686,.T.);
#10941=ORIENTED_EDGE('',*,*,#7725,.T.);
#10942=ORIENTED_EDGE('',*,*,#7661,.T.);
#10943=ORIENTED_EDGE('',*,*,#7621,.F.);
#10944=ORIENTED_EDGE('',*,*,#7675,.T.);
#10945=ORIENTED_EDGE('',*,*,#7726,.F.);
#10946=ORIENTED_EDGE('',*,*,#7623,.F.);
#10947=ORIENTED_EDGE('',*,*,#7727,.F.);
#10948=ORIENTED_EDGE('',*,*,#7580,.F.);
#10949=ORIENTED_EDGE('',*,*,#7658,.T.);
#10950=ORIENTED_EDGE('',*,*,#7657,.T.);
#10951=ORIENTED_EDGE('',*,*,#7654,.T.);
#10952=ORIENTED_EDGE('',*,*,#7651,.T.);
#10953=ORIENTED_EDGE('',*,*,#7648,.T.);
#10954=ORIENTED_EDGE('',*,*,#7645,.T.);
#10955=ORIENTED_EDGE('',*,*,#7642,.T.);
#10956=ORIENTED_EDGE('',*,*,#7639,.T.);
#10957=ORIENTED_EDGE('',*,*,#7636,.T.);
#10958=ORIENTED_EDGE('',*,*,#7633,.T.);
#10959=ORIENTED_EDGE('',*,*,#7630,.T.);
#10960=ORIENTED_EDGE('',*,*,#7627,.T.);
#10961=ORIENTED_EDGE('',*,*,#7624,.T.);
#10962=ORIENTED_EDGE('',*,*,#7726,.T.);
#10963=ORIENTED_EDGE('',*,*,#7579,.F.);
#10964=ORIENTED_EDGE('',*,*,#7583,.F.);
#10965=ORIENTED_EDGE('',*,*,#7586,.F.);
#10966=ORIENTED_EDGE('',*,*,#7589,.F.);
#10967=ORIENTED_EDGE('',*,*,#7592,.F.);
#10968=ORIENTED_EDGE('',*,*,#7595,.F.);
#10969=ORIENTED_EDGE('',*,*,#7598,.F.);
#10970=ORIENTED_EDGE('',*,*,#7601,.F.);
#10971=ORIENTED_EDGE('',*,*,#7604,.F.);
#10972=ORIENTED_EDGE('',*,*,#7607,.F.);
#10973=ORIENTED_EDGE('',*,*,#7610,.F.);
#10974=ORIENTED_EDGE('',*,*,#7613,.F.);
#10975=ORIENTED_EDGE('',*,*,#7616,.F.);
#10976=ORIENTED_EDGE('',*,*,#7728,.F.);
#10977=ORIENTED_EDGE('',*,*,#7676,.F.);
#10978=ORIENTED_EDGE('',*,*,#7673,.F.);
#10979=ORIENTED_EDGE('',*,*,#7615,.T.);
#10980=ORIENTED_EDGE('',*,*,#7729,.F.);
#10981=ORIENTED_EDGE('',*,*,#7677,.F.);
#10982=ORIENTED_EDGE('',*,*,#7728,.T.);
#10983=ORIENTED_EDGE('',*,*,#7729,.T.);
#10984=ORIENTED_EDGE('',*,*,#7617,.T.);
#10985=ORIENTED_EDGE('',*,*,#7614,.T.);
#10986=ORIENTED_EDGE('',*,*,#7611,.T.);
#10987=ORIENTED_EDGE('',*,*,#7608,.T.);
#10988=ORIENTED_EDGE('',*,*,#7605,.T.);
#10989=ORIENTED_EDGE('',*,*,#7602,.T.);
#10990=ORIENTED_EDGE('',*,*,#7599,.T.);
#10991=ORIENTED_EDGE('',*,*,#7596,.T.);
#10992=ORIENTED_EDGE('',*,*,#7593,.T.);
#10993=ORIENTED_EDGE('',*,*,#7590,.T.);
#10994=ORIENTED_EDGE('',*,*,#7587,.T.);
#10995=ORIENTED_EDGE('',*,*,#7584,.T.);
#10996=ORIENTED_EDGE('',*,*,#7581,.T.);
#10997=ORIENTED_EDGE('',*,*,#7727,.T.);
#10998=ORIENTED_EDGE('',*,*,#7622,.F.);
#10999=ORIENTED_EDGE('',*,*,#7619,.F.);
#11000=ORIENTED_EDGE('',*,*,#7626,.F.);
#11001=ORIENTED_EDGE('',*,*,#7629,.F.);
#11002=ORIENTED_EDGE('',*,*,#7632,.F.);
#11003=ORIENTED_EDGE('',*,*,#7635,.F.);
#11004=ORIENTED_EDGE('',*,*,#7638,.F.);
#11005=ORIENTED_EDGE('',*,*,#7641,.F.);
#11006=ORIENTED_EDGE('',*,*,#7644,.F.);
#11007=ORIENTED_EDGE('',*,*,#7647,.F.);
#11008=ORIENTED_EDGE('',*,*,#7650,.F.);
#11009=ORIENTED_EDGE('',*,*,#7653,.F.);
#11010=ORIENTED_EDGE('',*,*,#7656,.F.);
#11011=ORIENTED_EDGE('',*,*,#7660,.F.);
#11012=ORIENTED_EDGE('',*,*,#7678,.F.);
#11013=ORIENTED_EDGE('',*,*,#7722,.F.);
#11014=ORIENTED_EDGE('',*,*,#7689,.F.);
#11015=ORIENTED_EDGE('',*,*,#7724,.F.);
#11016=ORIENTED_EDGE('',*,*,#7710,.F.);
#11017=ORIENTED_EDGE('',*,*,#7692,.F.);
#11018=ORIENTED_EDGE('',*,*,#7680,.F.);
#11019=ORIENTED_EDGE('',*,*,#7707,.F.);
#11020=ORIENTED_EDGE('',*,*,#7681,.F.);
#11021=ORIENTED_EDGE('',*,*,#7683,.F.);
#11022=ORIENTED_EDGE('',*,*,#7713,.F.);
#11023=ORIENTED_EDGE('',*,*,#7714,.F.);
#11024=ORIENTED_EDGE('',*,*,#7695,.F.);
#11025=ORIENTED_EDGE('',*,*,#7717,.F.);
#11026=ORIENTED_EDGE('',*,*,#7708,.F.);
#11027=ORIENTED_EDGE('',*,*,#7719,.F.);
#11028=ORIENTED_EDGE('',*,*,#7699,.F.);
#11029=ORIENTED_EDGE('',*,*,#7715,.F.);
#11030=ORIENTED_EDGE('',*,*,#7703,.F.);
#11031=ORIENTED_EDGE('',*,*,#7723,.F.);
#11032=ORIENTED_EDGE('',*,*,#7705,.F.);
#11033=ORIENTED_EDGE('',*,*,#7725,.F.);
#11034=ORIENTED_EDGE('',*,*,#7685,.F.);
#11035=ORIENTED_EDGE('',*,*,#7730,.T.);
#11036=ORIENTED_EDGE('',*,*,#7731,.F.);
#11037=ORIENTED_EDGE('',*,*,#7732,.F.);
#11038=ORIENTED_EDGE('',*,*,#7733,.T.);
#11039=ORIENTED_EDGE('',*,*,#7734,.T.);
#11040=ORIENTED_EDGE('',*,*,#7735,.F.);
#11041=ORIENTED_EDGE('',*,*,#7730,.F.);
#11042=ORIENTED_EDGE('',*,*,#7736,.T.);
#11043=ORIENTED_EDGE('',*,*,#7737,.T.);
#11044=ORIENTED_EDGE('',*,*,#7738,.F.);
#11045=ORIENTED_EDGE('',*,*,#7734,.F.);
#11046=ORIENTED_EDGE('',*,*,#7739,.T.);
#11047=ORIENTED_EDGE('',*,*,#7740,.T.);
#11048=ORIENTED_EDGE('',*,*,#7741,.F.);
#11049=ORIENTED_EDGE('',*,*,#7737,.F.);
#11050=ORIENTED_EDGE('',*,*,#7742,.T.);
#11051=ORIENTED_EDGE('',*,*,#7743,.T.);
#11052=ORIENTED_EDGE('',*,*,#7744,.F.);
#11053=ORIENTED_EDGE('',*,*,#7740,.F.);
#11054=ORIENTED_EDGE('',*,*,#7745,.T.);
#11055=ORIENTED_EDGE('',*,*,#7746,.T.);
#11056=ORIENTED_EDGE('',*,*,#7747,.F.);
#11057=ORIENTED_EDGE('',*,*,#7743,.F.);
#11058=ORIENTED_EDGE('',*,*,#7748,.T.);
#11059=ORIENTED_EDGE('',*,*,#7749,.T.);
#11060=ORIENTED_EDGE('',*,*,#7750,.F.);
#11061=ORIENTED_EDGE('',*,*,#7746,.F.);
#11062=ORIENTED_EDGE('',*,*,#7751,.T.);
#11063=ORIENTED_EDGE('',*,*,#7752,.F.);
#11064=ORIENTED_EDGE('',*,*,#7753,.T.);
#11065=ORIENTED_EDGE('',*,*,#7754,.T.);
#11066=ORIENTED_EDGE('',*,*,#7755,.F.);
#11067=ORIENTED_EDGE('',*,*,#7756,.T.);
#11068=ORIENTED_EDGE('',*,*,#7757,.T.);
#11069=ORIENTED_EDGE('',*,*,#7758,.T.);
#11070=ORIENTED_EDGE('',*,*,#7759,.F.);
#11071=ORIENTED_EDGE('',*,*,#7760,.T.);
#11072=ORIENTED_EDGE('',*,*,#7761,.F.);
#11073=ORIENTED_EDGE('',*,*,#7760,.F.);
#11074=ORIENTED_EDGE('',*,*,#7762,.F.);
#11075=ORIENTED_EDGE('',*,*,#7763,.T.);
#11076=ORIENTED_EDGE('',*,*,#7764,.T.);
#11077=ORIENTED_EDGE('',*,*,#7756,.F.);
#11078=ORIENTED_EDGE('',*,*,#7765,.F.);
#11079=ORIENTED_EDGE('',*,*,#7766,.T.);
#11080=ORIENTED_EDGE('',*,*,#7767,.T.);
#11081=ORIENTED_EDGE('',*,*,#7763,.F.);
#11082=ORIENTED_EDGE('',*,*,#7768,.F.);
#11083=ORIENTED_EDGE('',*,*,#7769,.T.);
#11084=ORIENTED_EDGE('',*,*,#7770,.T.);
#11085=ORIENTED_EDGE('',*,*,#7766,.F.);
#11086=ORIENTED_EDGE('',*,*,#7771,.F.);
#11087=ORIENTED_EDGE('',*,*,#7772,.T.);
#11088=ORIENTED_EDGE('',*,*,#7773,.T.);
#11089=ORIENTED_EDGE('',*,*,#7769,.F.);
#11090=ORIENTED_EDGE('',*,*,#7774,.F.);
#11091=ORIENTED_EDGE('',*,*,#7775,.T.);
#11092=ORIENTED_EDGE('',*,*,#7776,.T.);
#11093=ORIENTED_EDGE('',*,*,#7772,.F.);
#11094=ORIENTED_EDGE('',*,*,#7777,.F.);
#11095=ORIENTED_EDGE('',*,*,#7778,.T.);
#11096=ORIENTED_EDGE('',*,*,#7779,.T.);
#11097=ORIENTED_EDGE('',*,*,#7775,.F.);
#11098=ORIENTED_EDGE('',*,*,#7780,.F.);
#11099=ORIENTED_EDGE('',*,*,#7781,.F.);
#11100=ORIENTED_EDGE('',*,*,#7782,.F.);
#11101=ORIENTED_EDGE('',*,*,#7783,.T.);
#11102=ORIENTED_EDGE('',*,*,#7784,.T.);
#11103=ORIENTED_EDGE('',*,*,#7781,.T.);
#11104=ORIENTED_EDGE('',*,*,#7785,.T.);
#11105=ORIENTED_EDGE('',*,*,#7778,.F.);
#11106=ORIENTED_EDGE('',*,*,#7786,.F.);
#11107=ORIENTED_EDGE('',*,*,#7787,.T.);
#11108=ORIENTED_EDGE('',*,*,#7788,.T.);
#11109=ORIENTED_EDGE('',*,*,#7789,.F.);
#11110=ORIENTED_EDGE('',*,*,#7788,.F.);
#11111=ORIENTED_EDGE('',*,*,#7790,.T.);
#11112=ORIENTED_EDGE('',*,*,#7791,.T.);
#11113=ORIENTED_EDGE('',*,*,#7792,.T.);
#11114=ORIENTED_EDGE('',*,*,#7793,.T.);
#11115=ORIENTED_EDGE('',*,*,#7794,.T.);
#11116=ORIENTED_EDGE('',*,*,#7795,.T.);
#11117=ORIENTED_EDGE('',*,*,#7796,.T.);
#11118=ORIENTED_EDGE('',*,*,#7797,.T.);
#11119=ORIENTED_EDGE('',*,*,#7798,.T.);
#11120=ORIENTED_EDGE('',*,*,#7799,.T.);
#11121=ORIENTED_EDGE('',*,*,#7800,.T.);
#11122=ORIENTED_EDGE('',*,*,#7801,.T.);
#11123=ORIENTED_EDGE('',*,*,#7732,.T.);
#11124=ORIENTED_EDGE('',*,*,#7802,.T.);
#11125=ORIENTED_EDGE('',*,*,#7783,.F.);
#11126=ORIENTED_EDGE('',*,*,#7803,.T.);
#11127=ORIENTED_EDGE('',*,*,#7789,.T.);
#11128=ORIENTED_EDGE('',*,*,#7804,.F.);
#11129=ORIENTED_EDGE('',*,*,#7805,.F.);
#11130=ORIENTED_EDGE('',*,*,#7806,.F.);
#11131=ORIENTED_EDGE('',*,*,#7807,.F.);
#11132=ORIENTED_EDGE('',*,*,#7808,.F.);
#11133=ORIENTED_EDGE('',*,*,#7809,.F.);
#11134=ORIENTED_EDGE('',*,*,#7787,.F.);
#11135=ORIENTED_EDGE('',*,*,#7761,.T.);
#11136=ORIENTED_EDGE('',*,*,#7810,.F.);
#11137=ORIENTED_EDGE('',*,*,#7790,.F.);
#11138=ORIENTED_EDGE('',*,*,#7811,.F.);
#11139=ORIENTED_EDGE('',*,*,#7812,.T.);
#11140=ORIENTED_EDGE('',*,*,#7804,.T.);
#11141=ORIENTED_EDGE('',*,*,#7813,.F.);
#11142=ORIENTED_EDGE('',*,*,#7814,.F.);
#11143=ORIENTED_EDGE('',*,*,#7813,.T.);
#11144=ORIENTED_EDGE('',*,*,#7809,.T.);
#11145=ORIENTED_EDGE('',*,*,#7815,.F.);
#11146=ORIENTED_EDGE('',*,*,#7816,.F.);
#11147=ORIENTED_EDGE('',*,*,#7792,.F.);
#11148=ORIENTED_EDGE('',*,*,#7817,.F.);
#11149=ORIENTED_EDGE('',*,*,#7794,.F.);
#11150=ORIENTED_EDGE('',*,*,#7818,.F.);
#11151=ORIENTED_EDGE('',*,*,#7815,.T.);
#11152=ORIENTED_EDGE('',*,*,#7808,.T.);
#11153=ORIENTED_EDGE('',*,*,#7819,.F.);
#11154=ORIENTED_EDGE('',*,*,#7820,.F.);
#11155=ORIENTED_EDGE('',*,*,#7819,.T.);
#11156=ORIENTED_EDGE('',*,*,#7807,.T.);
#11157=ORIENTED_EDGE('',*,*,#7821,.F.);
#11158=ORIENTED_EDGE('',*,*,#7822,.F.);
#11159=ORIENTED_EDGE('',*,*,#7796,.F.);
#11160=ORIENTED_EDGE('',*,*,#7823,.F.);
#11161=ORIENTED_EDGE('',*,*,#7798,.F.);
#11162=ORIENTED_EDGE('',*,*,#7824,.F.);
#11163=ORIENTED_EDGE('',*,*,#7821,.T.);
#11164=ORIENTED_EDGE('',*,*,#7806,.T.);
#11165=ORIENTED_EDGE('',*,*,#7825,.F.);
#11166=ORIENTED_EDGE('',*,*,#7826,.F.);
#11167=ORIENTED_EDGE('',*,*,#7800,.F.);
#11168=ORIENTED_EDGE('',*,*,#7827,.F.);
#11169=ORIENTED_EDGE('',*,*,#7825,.T.);
#11170=ORIENTED_EDGE('',*,*,#7805,.T.);
#11171=ORIENTED_EDGE('',*,*,#7812,.F.);
#11172=ORIENTED_EDGE('',*,*,#7754,.F.);
#11173=ORIENTED_EDGE('',*,*,#7828,.F.);
#11174=ORIENTED_EDGE('',*,*,#7758,.F.);
#11175=ORIENTED_EDGE('',*,*,#7829,.F.);
#11176=ORIENTED_EDGE('',*,*,#7752,.T.);
#11177=ORIENTED_EDGE('',*,*,#7830,.F.);
#11178=ORIENTED_EDGE('',*,*,#7749,.F.);
#11179=ORIENTED_EDGE('',*,*,#7831,.T.);
#11180=ORIENTED_EDGE('',*,*,#7731,.T.);
#11181=ORIENTED_EDGE('',*,*,#7735,.T.);
#11182=ORIENTED_EDGE('',*,*,#7738,.T.);
#11183=ORIENTED_EDGE('',*,*,#7741,.T.);
#11184=ORIENTED_EDGE('',*,*,#7744,.T.);
#11185=ORIENTED_EDGE('',*,*,#7747,.T.);
#11186=ORIENTED_EDGE('',*,*,#7750,.T.);
#11187=ORIENTED_EDGE('',*,*,#7830,.T.);
#11188=ORIENTED_EDGE('',*,*,#7755,.T.);
#11189=ORIENTED_EDGE('',*,*,#7829,.T.);
#11190=ORIENTED_EDGE('',*,*,#7757,.F.);
#11191=ORIENTED_EDGE('',*,*,#7764,.F.);
#11192=ORIENTED_EDGE('',*,*,#7767,.F.);
#11193=ORIENTED_EDGE('',*,*,#7770,.F.);
#11194=ORIENTED_EDGE('',*,*,#7773,.F.);
#11195=ORIENTED_EDGE('',*,*,#7776,.F.);
#11196=ORIENTED_EDGE('',*,*,#7779,.F.);
#11197=ORIENTED_EDGE('',*,*,#7785,.F.);
#11198=ORIENTED_EDGE('',*,*,#7784,.F.);
#11199=ORIENTED_EDGE('',*,*,#7802,.F.);
#11200=ORIENTED_EDGE('',*,*,#7782,.T.);
#11201=ORIENTED_EDGE('',*,*,#7786,.T.);
#11202=ORIENTED_EDGE('',*,*,#7780,.T.);
#11203=ORIENTED_EDGE('',*,*,#7777,.T.);
#11204=ORIENTED_EDGE('',*,*,#7774,.T.);
#11205=ORIENTED_EDGE('',*,*,#7771,.T.);
#11206=ORIENTED_EDGE('',*,*,#7768,.T.);
#11207=ORIENTED_EDGE('',*,*,#7765,.T.);
#11208=ORIENTED_EDGE('',*,*,#7762,.T.);
#11209=ORIENTED_EDGE('',*,*,#7759,.T.);
#11210=ORIENTED_EDGE('',*,*,#7828,.T.);
#11211=ORIENTED_EDGE('',*,*,#7753,.F.);
#11212=ORIENTED_EDGE('',*,*,#7831,.F.);
#11213=ORIENTED_EDGE('',*,*,#7751,.F.);
#11214=ORIENTED_EDGE('',*,*,#7748,.F.);
#11215=ORIENTED_EDGE('',*,*,#7745,.F.);
#11216=ORIENTED_EDGE('',*,*,#7742,.F.);
#11217=ORIENTED_EDGE('',*,*,#7739,.F.);
#11218=ORIENTED_EDGE('',*,*,#7736,.F.);
#11219=ORIENTED_EDGE('',*,*,#7733,.F.);
#11220=ORIENTED_EDGE('',*,*,#7803,.F.);
#11221=ORIENTED_EDGE('',*,*,#7797,.F.);
#11222=ORIENTED_EDGE('',*,*,#7822,.T.);
#11223=ORIENTED_EDGE('',*,*,#7824,.T.);
#11224=ORIENTED_EDGE('',*,*,#7793,.F.);
#11225=ORIENTED_EDGE('',*,*,#7816,.T.);
#11226=ORIENTED_EDGE('',*,*,#7818,.T.);
#11227=ORIENTED_EDGE('',*,*,#7795,.F.);
#11228=ORIENTED_EDGE('',*,*,#7817,.T.);
#11229=ORIENTED_EDGE('',*,*,#7820,.T.);
#11230=ORIENTED_EDGE('',*,*,#7799,.F.);
#11231=ORIENTED_EDGE('',*,*,#7823,.T.);
#11232=ORIENTED_EDGE('',*,*,#7827,.T.);
#11233=ORIENTED_EDGE('',*,*,#7801,.F.);
#11234=ORIENTED_EDGE('',*,*,#7826,.T.);
#11235=ORIENTED_EDGE('',*,*,#7811,.T.);
#11236=ORIENTED_EDGE('',*,*,#7791,.F.);
#11237=ORIENTED_EDGE('',*,*,#7810,.T.);
#11238=ORIENTED_EDGE('',*,*,#7814,.T.);
#11239=ORIENTED_EDGE('',*,*,#7832,.F.);
#11240=ORIENTED_EDGE('',*,*,#7833,.T.);
#11241=ORIENTED_EDGE('',*,*,#7834,.F.);
#11242=ORIENTED_EDGE('',*,*,#7833,.F.);
#11243=ORIENTED_EDGE('',*,*,#7835,.F.);
#11244=ORIENTED_EDGE('',*,*,#7836,.F.);
#11245=ORIENTED_EDGE('',*,*,#7837,.T.);
#11246=ORIENTED_EDGE('',*,*,#7838,.F.);
#11247=ORIENTED_EDGE('',*,*,#7837,.F.);
#11248=ORIENTED_EDGE('',*,*,#7839,.T.);
#11249=ORIENTED_EDGE('',*,*,#7840,.T.);
#11250=ORIENTED_EDGE('',*,*,#7832,.T.);
#11251=ORIENTED_EDGE('',*,*,#7840,.F.);
#11252=ORIENTED_EDGE('',*,*,#7835,.T.);
#11253=ORIENTED_EDGE('',*,*,#7836,.T.);
#11254=ORIENTED_EDGE('',*,*,#7841,.T.);
#11255=ORIENTED_EDGE('',*,*,#7842,.F.);
#11256=ORIENTED_EDGE('',*,*,#7841,.F.);
#11257=ORIENTED_EDGE('',*,*,#7838,.T.);
#11258=ORIENTED_EDGE('',*,*,#7834,.T.);
#11259=ORIENTED_EDGE('',*,*,#7839,.F.);
#11260=ORIENTED_EDGE('',*,*,#7842,.T.);
#11261=ORIENTED_EDGE('',*,*,#7843,.F.);
#11262=ORIENTED_EDGE('',*,*,#7844,.T.);
#11263=ORIENTED_EDGE('',*,*,#7845,.F.);
#11264=ORIENTED_EDGE('',*,*,#7844,.F.);
#11265=ORIENTED_EDGE('',*,*,#7846,.F.);
#11266=ORIENTED_EDGE('',*,*,#7847,.F.);
#11267=ORIENTED_EDGE('',*,*,#7848,.T.);
#11268=ORIENTED_EDGE('',*,*,#7849,.F.);
#11269=ORIENTED_EDGE('',*,*,#7848,.F.);
#11270=ORIENTED_EDGE('',*,*,#7846,.T.);
#11271=ORIENTED_EDGE('',*,*,#7847,.T.);
#11272=ORIENTED_EDGE('',*,*,#7850,.T.);
#11273=ORIENTED_EDGE('',*,*,#7843,.T.);
#11274=ORIENTED_EDGE('',*,*,#7850,.F.);
#11275=ORIENTED_EDGE('',*,*,#7845,.T.);
#11276=ORIENTED_EDGE('',*,*,#7849,.T.);
#11277=CONICAL_SURFACE('',#12300,13.,0.785398163397443);
#11278=CONICAL_SURFACE('',#12303,12.4000000000001,0.785398163397443);
#11279=CONICAL_SURFACE('',#12306,13.,0.785398163397454);
#11280=CONICAL_SURFACE('',#12309,16.,0.785398163397466);
#11281=CONICAL_SURFACE('',#12312,12.4000000000001,0.785398163397443);
#11282=CONICAL_SURFACE('',#12315,15.4,0.785398163397495);
#11283=CONICAL_SURFACE('',#12694,14.7,0.785398163397379);
#11284=CONICAL_SURFACE('',#12697,15.,0.785398163397457);
#11285=CONICAL_SURFACE('',#12750,7.39999999999998,0.785398163397459);
#11286=CONICAL_SURFACE('',#12753,12.5,0.785398163397438);
#11287=CONICAL_SURFACE('',#12756,13.,0.785398163397455);
#11288=CONICAL_SURFACE('',#12766,7.39999999999998,0.785398163397459);
#11289=CONICAL_SURFACE('',#12769,12.5,0.785398163397438);
#11290=CONICAL_SURFACE('',#12772,13.,0.785398163397455);
#11291=CONICAL_SURFACE('',#12786,10.5,0.785398163397448);
#11292=CONICAL_SURFACE('',#12790,37.1705339516543,0.785398163397448);
#11293=CONICAL_SURFACE('',#12828,32.2782665420145,0.872664625997169);
#11294=CONICAL_SURFACE('',#12830,32.2782665420145,0.872664625997169);
#11295=CONICAL_SURFACE('',#12832,32.2782665420145,0.872664625997169);
#11296=CONICAL_SURFACE('',#12835,32.2782665420145,0.872664625997169);
#11297=CONICAL_SURFACE('',#12856,37.1705339516543,0.785398163397448);
#11298=CONICAL_SURFACE('',#12857,37.1705339516543,0.785398163397448);
#11299=CONICAL_SURFACE('',#12858,37.1705339516543,0.785398163397448);
#11300=CONICAL_SURFACE('',#12860,13.5,0.785398163397453);
#11301=CONICAL_SURFACE('',#12945,7.,0.785398163397443);
#11302=CONICAL_SURFACE('',#12948,8.00000000000001,0.785398163397448);
#11303=CONICAL_SURFACE('',#12955,7.,0.785398163397445);
#11304=CONICAL_SURFACE('',#12958,8.,0.785398163397455);
#11305=CONICAL_SURFACE('',#13056,27.,0.158655262186402);
#11306=CONICAL_SURFACE('',#13165,14.,0.785398163397448);
#11307=CONICAL_SURFACE('',#13174,7.50000000000001,1.13838855122436);
#11308=CONICAL_SURFACE('',#13265,4.,0.5235987755983);
#11309=CONICAL_SURFACE('',#13278,5.99999999999997,0.78539816339745);
#11310=CONICAL_SURFACE('',#13284,4.00000000000001,0.5235987755983);
#11311=CONICAL_SURFACE('',#13297,5.99999999999998,0.78539816339745);
#11312=CONICAL_SURFACE('',#13457,5.49999999999999,0.785398163397442);
#11313=CONICAL_SURFACE('',#13460,6.,0.785398163397442);
#11314=CONICAL_SURFACE('',#13468,20.6,0.785398163397443);
#11315=CONICAL_SURFACE('',#13472,20.,0.785398163397457);
#11316=CONICAL_SURFACE('',#13497,7.00000000000002,1.05840686648416);
#11317=CONICAL_SURFACE('',#13501,15.,1.05840686648416);
#11318=CONICAL_SURFACE('',#13516,20.6,0.785398163397443);
#11319=CONICAL_SURFACE('',#13520,20.,0.785398163397457);
#11320=CONICAL_SURFACE('',#13545,7.,1.05840686648416);
#11321=CONICAL_SURFACE('',#13549,15.,1.05840686648416);
#11322=CONICAL_SURFACE('',#13560,4.90000000000001,0.785398163397295);
#11323=CONICAL_SURFACE('',#13563,4.7,0.785398163397478);
#11324=CONICAL_SURFACE('',#13610,4.35000000000001,0.785398163397442);
#11325=CONICAL_SURFACE('',#13694,9.70000000000001,0.785398163397434);
#11326=CONICAL_SURFACE('',#13697,6.,0.785398163397452);
#11327=CONICAL_SURFACE('',#13709,6.49999999999999,0.785398163397442);
#11328=CONICAL_SURFACE('',#13712,7.50000000000001,0.785398163397452);
#11329=ADVANCED_FACE('',(#1247),#11277,.T.);
#11330=ADVANCED_FACE('',(#1248),#11278,.T.);
#11331=ADVANCED_FACE('',(#1249),#11279,.T.);
#11332=ADVANCED_FACE('',(#1250),#11280,.T.);
#11333=ADVANCED_FACE('',(#1251),#11281,.T.);
#11334=ADVANCED_FACE('',(#1252),#11282,.T.);
#11335=ADVANCED_FACE('',(#1253),#975,.F.);
#11336=ADVANCED_FACE('',(#1254),#811,.T.);
#11337=ADVANCED_FACE('',(#1255),#812,.F.);
#11338=ADVANCED_FACE('',(#1256),#813,.F.);
#11339=ADVANCED_FACE('',(#1257),#814,.F.);
#11340=ADVANCED_FACE('',(#1258),#815,.F.);
#11341=ADVANCED_FACE('',(#1259),#816,.F.);
#11342=ADVANCED_FACE('',(#1260),#817,.F.);
#11343=ADVANCED_FACE('',(#1261),#818,.F.);
#11344=ADVANCED_FACE('',(#1262),#819,.F.);
#11345=ADVANCED_FACE('',(#1263),#820,.F.);
#11346=ADVANCED_FACE('',(#1264),#821,.F.);
#11347=ADVANCED_FACE('',(#1265),#976,.F.);
#11348=ADVANCED_FACE('',(#1266),#822,.F.);
#11349=ADVANCED_FACE('',(#1267),#977,.F.);
#11350=ADVANCED_FACE('',(#1268),#978,.T.);
#11351=ADVANCED_FACE('',(#1269),#979,.T.);
#11352=ADVANCED_FACE('',(#1270),#980,.T.);
#11353=ADVANCED_FACE('',(#1271),#981,.F.);
#11354=ADVANCED_FACE('',(#1272),#982,.T.);
#11355=ADVANCED_FACE('',(#1273),#983,.F.);
#11356=ADVANCED_FACE('',(#1274),#984,.F.);
#11357=ADVANCED_FACE('',(#1275),#985,.F.);
#11358=ADVANCED_FACE('',(#1276),#986,.T.);
#11359=ADVANCED_FACE('',(#1277),#987,.T.);
#11360=ADVANCED_FACE('',(#1278),#988,.T.);
#11361=ADVANCED_FACE('',(#1279),#989,.T.);
#11362=ADVANCED_FACE('',(#1280),#990,.F.);
#11363=ADVANCED_FACE('',(#1281),#991,.F.);
#11364=ADVANCED_FACE('',(#1282),#992,.F.);
#11365=ADVANCED_FACE('',(#1283),#993,.T.);
#11366=ADVANCED_FACE('',(#1284),#994,.F.);
#11367=ADVANCED_FACE('',(#1285),#995,.T.);
#11368=ADVANCED_FACE('',(#1286),#996,.F.);
#11369=ADVANCED_FACE('',(#1287),#448,.T.);
#11370=ADVANCED_FACE('',(#1288),#449,.T.);
#11371=ADVANCED_FACE('',(#1289),#450,.T.);
#11372=ADVANCED_FACE('',(#1290),#451,.F.);
#11373=ADVANCED_FACE('',(#1291),#452,.F.);
#11374=ADVANCED_FACE('',(#1292),#453,.F.);
#11375=ADVANCED_FACE('',(#1293),#997,.T.);
#11376=ADVANCED_FACE('',(#1294),#454,.F.);
#11377=ADVANCED_FACE('',(#1295),#455,.T.);
#11378=ADVANCED_FACE('',(#1296),#456,.T.);
#11379=ADVANCED_FACE('',(#1297),#998,.F.);
#11380=ADVANCED_FACE('',(#1298),#999,.F.);
#11381=ADVANCED_FACE('',(#1299),#457,.T.);
#11382=ADVANCED_FACE('',(#1300),#458,.T.);
#11383=ADVANCED_FACE('',(#1301),#459,.F.);
#11384=ADVANCED_FACE('',(#1302),#460,.F.);
#11385=ADVANCED_FACE('',(#1303,#335,#336,#337,#338,#339),#461,.T.);
#11386=ADVANCED_FACE('',(#1304,#340,#341,#342),#462,.F.);
#11387=ADVANCED_FACE('',(#1305),#463,.F.);
#11388=ADVANCED_FACE('',(#1306),#464,.F.);
#11389=ADVANCED_FACE('',(#1307),#1000,.F.);
#11390=ADVANCED_FACE('',(#1308,#343,#344,#345,#346,#347),#465,.T.);
#11391=ADVANCED_FACE('',(#1309),#466,.F.);
#11392=ADVANCED_FACE('',(#1310),#467,.F.);
#11393=ADVANCED_FACE('',(#1311),#468,.F.);
#11394=ADVANCED_FACE('',(#1312),#469,.F.);
#11395=ADVANCED_FACE('',(#1313,#348),#470,.T.);
#11396=ADVANCED_FACE('',(#1314),#471,.T.);
#11397=ADVANCED_FACE('',(#1315),#1001,.T.);
#11398=ADVANCED_FACE('',(#1316),#472,.T.);
#11399=ADVANCED_FACE('',(#1317,#349),#473,.F.);
#11400=ADVANCED_FACE('',(#1318),#474,.F.);
#11401=ADVANCED_FACE('',(#1319),#1002,.F.);
#11402=ADVANCED_FACE('',(#1320),#475,.F.);
#11403=ADVANCED_FACE('',(#1321,#350),#476,.T.);
#11404=ADVANCED_FACE('',(#1322),#477,.F.);
#11405=ADVANCED_FACE('',(#1323),#1003,.F.);
#11406=ADVANCED_FACE('',(#1324),#478,.F.);
#11407=ADVANCED_FACE('',(#1325),#479,.F.);
#11408=ADVANCED_FACE('',(#1326),#1004,.T.);
#11409=ADVANCED_FACE('',(#1327),#1005,.T.);
#11410=ADVANCED_FACE('',(#1328),#1006,.T.);
#11411=ADVANCED_FACE('',(#1329),#1007,.T.);
#11412=ADVANCED_FACE('',(#1330),#1008,.T.);
#11413=ADVANCED_FACE('',(#1331),#480,.F.);
#11414=ADVANCED_FACE('',(#1332),#481,.F.);
#11415=ADVANCED_FACE('',(#1333),#482,.F.);
#11416=ADVANCED_FACE('',(#1334),#483,.F.);
#11417=ADVANCED_FACE('',(#1335),#484,.F.);
#11418=ADVANCED_FACE('',(#1336),#485,.T.);
#11419=ADVANCED_FACE('',(#1337,#351),#486,.T.);
#11420=ADVANCED_FACE('',(#1338,#352),#487,.T.);
#11421=ADVANCED_FACE('',(#1339,#353),#488,.T.);
#11422=ADVANCED_FACE('',(#1340),#489,.T.);
#11423=ADVANCED_FACE('',(#1341),#490,.T.);
#11424=ADVANCED_FACE('',(#1342),#491,.T.);
#11425=ADVANCED_FACE('',(#1343),#492,.T.);
#11426=ADVANCED_FACE('',(#1344,#354,#355,#356),#493,.F.);
#11427=ADVANCED_FACE('',(#1345,#357),#494,.T.);
#11428=ADVANCED_FACE('',(#1346,#358),#495,.F.);
#11429=ADVANCED_FACE('',(#1347),#496,.T.);
#11430=ADVANCED_FACE('',(#1348),#497,.T.);
#11431=ADVANCED_FACE('',(#1349),#498,.T.);
#11432=ADVANCED_FACE('',(#1350,#359),#499,.T.);
#11433=ADVANCED_FACE('',(#1351),#1009,.T.);
#11434=ADVANCED_FACE('',(#1352),#1010,.T.);
#11435=ADVANCED_FACE('',(#1353),#1011,.T.);
#11436=ADVANCED_FACE('',(#1354),#1012,.T.);
#11437=ADVANCED_FACE('',(#1355),#500,.T.);
#11438=ADVANCED_FACE('',(#1356),#501,.T.);
#11439=ADVANCED_FACE('',(#1357),#502,.T.);
#11440=ADVANCED_FACE('',(#1358),#503,.T.);
#11441=ADVANCED_FACE('',(#1359),#504,.T.);
#11442=ADVANCED_FACE('',(#1360,#360),#505,.T.);
#11443=ADVANCED_FACE('',(#1361,#361),#506,.T.);
#11444=ADVANCED_FACE('',(#1362,#362),#507,.T.);
#11445=ADVANCED_FACE('',(#1363),#508,.T.);
#11446=ADVANCED_FACE('',(#1364),#509,.T.);
#11447=ADVANCED_FACE('',(#1365),#510,.T.);
#11448=ADVANCED_FACE('',(#1366),#511,.T.);
#11449=ADVANCED_FACE('',(#1367),#512,.F.);
#11450=ADVANCED_FACE('',(#1368),#513,.T.);
#11451=ADVANCED_FACE('',(#1369),#1013,.T.);
#11452=ADVANCED_FACE('',(#1370),#1014,.T.);
#11453=ADVANCED_FACE('',(#1371),#1015,.T.);
#11454=ADVANCED_FACE('',(#1372),#1016,.T.);
#11455=ADVANCED_FACE('',(#1373),#1017,.F.);
#11456=ADVANCED_FACE('',(#1374),#1018,.F.);
#11457=ADVANCED_FACE('',(#1375),#1019,.F.);
#11458=ADVANCED_FACE('',(#1376),#1020,.F.);
#11459=ADVANCED_FACE('',(#1377),#1021,.F.);
#11460=ADVANCED_FACE('',(#1378),#1022,.F.);
#11461=ADVANCED_FACE('',(#1379),#327,.F.);
#11462=ADVANCED_FACE('',(#1380),#328,.F.);
#11463=ADVANCED_FACE('',(#1381),#1023,.F.);
#11464=ADVANCED_FACE('',(#1382),#1024,.F.);
#11465=ADVANCED_FACE('',(#1383),#823,.F.);
#11466=ADVANCED_FACE('',(#1384),#1025,.T.);
#11467=ADVANCED_FACE('',(#1385),#1026,.T.);
#11468=ADVANCED_FACE('',(#1386),#1027,.F.);
#11469=ADVANCED_FACE('',(#1387),#1028,.F.);
#11470=ADVANCED_FACE('',(#1388),#1029,.T.);
#11471=ADVANCED_FACE('',(#1389),#1030,.T.);
#11472=ADVANCED_FACE('',(#1390),#1031,.F.);
#11473=ADVANCED_FACE('',(#1391),#1032,.F.);
#11474=ADVANCED_FACE('',(#1392),#1033,.T.);
#11475=ADVANCED_FACE('',(#1393),#1034,.T.);
#11476=ADVANCED_FACE('',(#1394),#308,.F.);
#11477=ADVANCED_FACE('',(#1395),#309,.F.);
#11478=ADVANCED_FACE('',(#1396),#1035,.T.);
#11479=ADVANCED_FACE('',(#1397),#1036,.T.);
#11480=ADVANCED_FACE('',(#1398),#1037,.T.);
#11481=ADVANCED_FACE('',(#1399),#824,.T.);
#11482=ADVANCED_FACE('',(#1400),#1038,.T.);
#11483=ADVANCED_FACE('',(#1401),#1039,.F.);
#11484=ADVANCED_FACE('',(#1402),#1040,.F.);
#11485=ADVANCED_FACE('',(#1403),#1041,.F.);
#11486=ADVANCED_FACE('',(#1404),#1042,.F.);
#11487=ADVANCED_FACE('',(#1405),#1043,.F.);
#11488=ADVANCED_FACE('',(#1406),#1044,.F.);
#11489=ADVANCED_FACE('',(#1407),#1045,.F.);
#11490=ADVANCED_FACE('',(#1408),#1046,.T.);
#11491=ADVANCED_FACE('',(#1409),#1047,.T.);
#11492=ADVANCED_FACE('',(#1410),#1048,.T.);
#11493=ADVANCED_FACE('',(#1411,#363,#364),#514,.F.);
#11494=ADVANCED_FACE('',(#1412),#515,.F.);
#11495=ADVANCED_FACE('',(#1413),#1049,.T.);
#11496=ADVANCED_FACE('',(#1414,#365,#366,#367),#516,.F.);
#11497=ADVANCED_FACE('',(#1415),#517,.F.);
#11498=ADVANCED_FACE('',(#1416),#1050,.F.);
#11499=ADVANCED_FACE('',(#1417),#518,.F.);
#11500=ADVANCED_FACE('',(#1418),#1051,.F.);
#11501=ADVANCED_FACE('',(#1419),#519,.F.);
#11502=ADVANCED_FACE('',(#1420),#520,.F.);
#11503=ADVANCED_FACE('',(#1421,#368,#369),#521,.T.);
#11504=ADVANCED_FACE('',(#1422),#522,.F.);
#11505=ADVANCED_FACE('',(#1423),#11283,.T.);
#11506=ADVANCED_FACE('',(#1424),#11284,.T.);
#11507=ADVANCED_FACE('',(#1425),#825,.F.);
#11508=ADVANCED_FACE('',(#1426),#826,.F.);
#11509=ADVANCED_FACE('',(#1427),#1052,.F.);
#11510=ADVANCED_FACE('',(#1428),#1053,.F.);
#11511=ADVANCED_FACE('',(#1429),#1054,.F.);
#11512=ADVANCED_FACE('',(#1430),#1055,.T.);
#11513=ADVANCED_FACE('',(#1431),#1056,.F.);
#11514=ADVANCED_FACE('',(#1432),#1057,.F.);
#11515=ADVANCED_FACE('',(#1433),#1058,.F.);
#11516=ADVANCED_FACE('',(#1434),#1059,.T.);
#11517=ADVANCED_FACE('',(#1435),#523,.F.);
#11518=ADVANCED_FACE('',(#1436),#1060,.T.);
#11519=ADVANCED_FACE('',(#1437),#1061,.T.);
#11520=ADVANCED_FACE('',(#1438),#524,.F.);
#11521=ADVANCED_FACE('',(#1439),#525,.F.);
#11522=ADVANCED_FACE('',(#1440),#526,.F.);
#11523=ADVANCED_FACE('',(#1441),#527,.F.);
#11524=ADVANCED_FACE('',(#1442),#528,.F.);
#11525=ADVANCED_FACE('',(#1443),#529,.F.);
#11526=ADVANCED_FACE('',(#1444),#530,.F.);
#11527=ADVANCED_FACE('',(#1445,#370,#371,#372),#531,.F.);
#11528=ADVANCED_FACE('',(#1446,#373),#532,.T.);
#11529=ADVANCED_FACE('',(#1447,#374),#533,.T.);
#11530=ADVANCED_FACE('',(#1448),#1062,.T.);
#11531=ADVANCED_FACE('',(#1449),#1063,.T.);
#11532=ADVANCED_FACE('',(#1450),#534,.T.);
#11533=ADVANCED_FACE('',(#1451),#535,.T.);
#11534=ADVANCED_FACE('',(#1452),#1064,.T.);
#11535=ADVANCED_FACE('',(#1453),#1065,.T.);
#11536=ADVANCED_FACE('',(#1454),#1066,.F.);
#11537=ADVANCED_FACE('',(#1455),#1067,.F.);
#11538=ADVANCED_FACE('',(#1456),#11285,.T.);
#11539=ADVANCED_FACE('',(#1457),#11286,.T.);
#11540=ADVANCED_FACE('',(#1458),#11287,.T.);
#11541=ADVANCED_FACE('',(#1459),#1068,.T.);
#11542=ADVANCED_FACE('',(#1460),#1069,.T.);
#11543=ADVANCED_FACE('',(#1461),#536,.T.);
#11544=ADVANCED_FACE('',(#1462,#375),#537,.F.);
#11545=ADVANCED_FACE('',(#1463),#538,.T.);
#11546=ADVANCED_FACE('',(#1464),#11288,.T.);
#11547=ADVANCED_FACE('',(#1465),#11289,.T.);
#11548=ADVANCED_FACE('',(#1466),#11290,.T.);
#11549=ADVANCED_FACE('',(#1467),#1070,.T.);
#11550=ADVANCED_FACE('',(#1468),#1071,.T.);
#11551=ADVANCED_FACE('',(#1469),#539,.T.);
#11552=ADVANCED_FACE('',(#1470,#376),#540,.F.);
#11553=ADVANCED_FACE('',(#1471),#541,.T.);
#11554=ADVANCED_FACE('',(#1472),#11291,.T.);
#11555=ADVANCED_FACE('',(#1473),#11292,.T.);
#11556=ADVANCED_FACE('',(#1474),#329,.F.);
#11557=ADVANCED_FACE('',(#1475,#377),#330,.T.);
#11558=ADVANCED_FACE('',(#1476),#1072,.T.);
#11559=ADVANCED_FACE('',(#1477),#11293,.T.);
#11560=ADVANCED_FACE('',(#1478),#11294,.T.);
#11561=ADVANCED_FACE('',(#1479),#11295,.T.);
#11562=ADVANCED_FACE('',(#1480),#542,.F.);
#11563=ADVANCED_FACE('',(#1481),#11296,.T.);
#11564=ADVANCED_FACE('',(#1482),#543,.F.);
#11565=ADVANCED_FACE('',(#1483),#544,.F.);
#11566=ADVANCED_FACE('',(#1484),#545,.F.);
#11567=ADVANCED_FACE('',(#1485),#546,.F.);
#11568=ADVANCED_FACE('',(#1486),#547,.F.);
#11569=ADVANCED_FACE('',(#1487),#548,.F.);
#11570=ADVANCED_FACE('',(#1488),#549,.F.);
#11571=ADVANCED_FACE('',(#1489),#550,.F.);
#11572=ADVANCED_FACE('',(#1490),#551,.F.);
#11573=ADVANCED_FACE('',(#1491),#552,.F.);
#11574=ADVANCED_FACE('',(#1492),#553,.F.);
#11575=ADVANCED_FACE('',(#1493),#554,.F.);
#11576=ADVANCED_FACE('',(#1494),#555,.F.);
#11577=ADVANCED_FACE('',(#1495),#556,.F.);
#11578=ADVANCED_FACE('',(#1496),#557,.F.);
#11579=ADVANCED_FACE('',(#1497),#558,.F.);
#11580=ADVANCED_FACE('',(#1498),#11297,.T.);
#11581=ADVANCED_FACE('',(#1499),#11298,.T.);
#11582=ADVANCED_FACE('',(#1500),#11299,.T.);
#11583=ADVANCED_FACE('',(#1501),#11300,.F.);
#11584=ADVANCED_FACE('',(#1502),#827,.F.);
#11585=ADVANCED_FACE('',(#1503),#828,.F.);
#11586=ADVANCED_FACE('',(#1504),#1073,.T.);
#11587=ADVANCED_FACE('',(#1505),#1074,.F.);
#11588=ADVANCED_FACE('',(#1506),#1075,.T.);
#11589=ADVANCED_FACE('',(#1507),#1076,.F.);
#11590=ADVANCED_FACE('',(#1508),#1077,.F.);
#11591=ADVANCED_FACE('',(#1509),#1078,.F.);
#11592=ADVANCED_FACE('',(#1510),#1079,.F.);
#11593=ADVANCED_FACE('',(#1511),#1080,.T.);
#11594=ADVANCED_FACE('',(#1512),#1081,.F.);
#11595=ADVANCED_FACE('',(#1513),#1082,.T.);
#11596=ADVANCED_FACE('',(#1514),#1083,.F.);
#11597=ADVANCED_FACE('',(#1515),#559,.F.);
#11598=ADVANCED_FACE('',(#1516),#1084,.F.);
#11599=ADVANCED_FACE('',(#1517),#560,.F.);
#11600=ADVANCED_FACE('',(#1518),#561,.F.);
#11601=ADVANCED_FACE('',(#1519,#378,#379),#562,.T.);
#11602=ADVANCED_FACE('',(#1520,#380,#381),#563,.F.);
#11603=ADVANCED_FACE('',(#1521,#382),#564,.F.);
#11604=ADVANCED_FACE('',(#1522,#383),#565,.F.);
#11605=ADVANCED_FACE('',(#1523),#566,.F.);
#11606=ADVANCED_FACE('',(#1524),#567,.F.);
#11607=ADVANCED_FACE('',(#1525,#384),#568,.F.);
#11608=ADVANCED_FACE('',(#1526),#1085,.T.);
#11609=ADVANCED_FACE('',(#1527),#1086,.T.);
#11610=ADVANCED_FACE('',(#1528,#385),#569,.F.);
#11611=ADVANCED_FACE('',(#1529,#386,#387),#570,.F.);
#11612=ADVANCED_FACE('',(#1530,#388,#389),#571,.F.);
#11613=ADVANCED_FACE('',(#1531,#390),#572,.F.);
#11614=ADVANCED_FACE('',(#1532),#573,.F.);
#11615=ADVANCED_FACE('',(#1533),#574,.F.);
#11616=ADVANCED_FACE('',(#1534),#575,.F.);
#11617=ADVANCED_FACE('',(#1535,#391),#576,.F.);
#11618=ADVANCED_FACE('',(#1536,#392),#577,.T.);
#11619=ADVANCED_FACE('',(#1537),#1087,.F.);
#11620=ADVANCED_FACE('',(#1538),#1088,.F.);
#11621=ADVANCED_FACE('',(#1539),#1089,.T.);
#11622=ADVANCED_FACE('',(#1540),#1090,.T.);
#11623=ADVANCED_FACE('',(#1541),#11301,.T.);
#11624=ADVANCED_FACE('',(#1542),#11302,.T.);
#11625=ADVANCED_FACE('',(#1543),#1091,.T.);
#11626=ADVANCED_FACE('',(#1544),#578,.T.);
#11627=ADVANCED_FACE('',(#1545),#579,.F.);
#11628=ADVANCED_FACE('',(#1546),#11303,.T.);
#11629=ADVANCED_FACE('',(#1547),#11304,.T.);
#11630=ADVANCED_FACE('',(#1548),#1092,.T.);
#11631=ADVANCED_FACE('',(#1549),#580,.T.);
#11632=ADVANCED_FACE('',(#1550),#581,.F.);
#11633=ADVANCED_FACE('',(#1551),#1093,.F.);
#11634=ADVANCED_FACE('',(#1552),#1094,.F.);
#11635=ADVANCED_FACE('',(#1553,#393,#394),#582,.T.);
#11636=ADVANCED_FACE('',(#1554,#395,#396),#583,.F.);
#11637=ADVANCED_FACE('',(#1555),#584,.F.);
#11638=ADVANCED_FACE('',(#1556),#585,.F.);
#11639=ADVANCED_FACE('',(#1557),#586,.F.);
#11640=ADVANCED_FACE('',(#1558),#587,.F.);
#11641=ADVANCED_FACE('',(#1559),#1095,.T.);
#11642=ADVANCED_FACE('',(#1560),#1096,.T.);
#11643=ADVANCED_FACE('',(#1561),#1097,.T.);
#11644=ADVANCED_FACE('',(#1562),#1098,.T.);
#11645=ADVANCED_FACE('',(#1563),#1099,.F.);
#11646=ADVANCED_FACE('',(#1564),#829,.T.);
#11647=ADVANCED_FACE('',(#1565),#830,.T.);
#11648=ADVANCED_FACE('',(#1566),#1100,.F.);
#11649=ADVANCED_FACE('',(#1567,#397),#1101,.F.);
#11650=ADVANCED_FACE('',(#1568),#1102,.F.);
#11651=ADVANCED_FACE('',(#1569),#1103,.F.);
#11652=ADVANCED_FACE('',(#1570),#1104,.T.);
#11653=ADVANCED_FACE('',(#1571),#1105,.T.);
#11654=ADVANCED_FACE('',(#1572),#1106,.T.);
#11655=ADVANCED_FACE('',(#1573),#1107,.T.);
#11656=ADVANCED_FACE('',(#1574),#1108,.T.);
#11657=ADVANCED_FACE('',(#1575),#1109,.T.);
#11658=ADVANCED_FACE('',(#1576),#1110,.T.);
#11659=ADVANCED_FACE('',(#1577),#1111,.T.);
#11660=ADVANCED_FACE('',(#1578),#11305,.T.);
#11661=ADVANCED_FACE('',(#1579),#1112,.T.);
#11662=ADVANCED_FACE('',(#1580,#398),#588,.F.);
#11663=ADVANCED_FACE('',(#1581),#1113,.F.);
#11664=ADVANCED_FACE('',(#1582),#589,.F.);
#11665=ADVANCED_FACE('',(#1583,#399),#590,.T.);
#11666=ADVANCED_FACE('',(#1584,#400),#591,.F.);
#11667=ADVANCED_FACE('',(#1585),#592,.T.);
#11668=ADVANCED_FACE('',(#1586),#593,.T.);
#11669=ADVANCED_FACE('',(#1587,#401),#594,.T.);
#11670=ADVANCED_FACE('',(#1588,#402),#595,.T.);
#11671=ADVANCED_FACE('',(#1589,#403),#596,.T.);
#11672=ADVANCED_FACE('',(#1590,#404),#597,.T.);
#11673=ADVANCED_FACE('',(#1591),#598,.F.);
#11674=ADVANCED_FACE('',(#1592),#599,.F.);
#11675=ADVANCED_FACE('',(#1593),#600,.F.);
#11676=ADVANCED_FACE('',(#1594),#601,.F.);
#11677=ADVANCED_FACE('',(#1595),#602,.F.);
#11678=ADVANCED_FACE('',(#1596),#603,.F.);
#11679=ADVANCED_FACE('',(#1597,#405),#604,.T.);
#11680=ADVANCED_FACE('',(#1598),#605,.T.);
#11681=ADVANCED_FACE('',(#1599),#606,.F.);
#11682=ADVANCED_FACE('',(#1600,#406),#607,.F.);
#11683=ADVANCED_FACE('',(#1601,#407),#608,.F.);
#11684=ADVANCED_FACE('',(#1602),#609,.F.);
#11685=ADVANCED_FACE('',(#1603),#610,.F.);
#11686=ADVANCED_FACE('',(#1604),#611,.F.);
#11687=ADVANCED_FACE('',(#1605),#612,.F.);
#11688=ADVANCED_FACE('',(#1606),#613,.F.);
#11689=ADVANCED_FACE('',(#1607),#614,.F.);
#11690=ADVANCED_FACE('',(#1608),#615,.F.);
#11691=ADVANCED_FACE('',(#1609),#616,.F.);
#11692=ADVANCED_FACE('',(#1610),#617,.F.);
#11693=ADVANCED_FACE('',(#1611),#618,.F.);
#11694=ADVANCED_FACE('',(#1612),#619,.F.);
#11695=ADVANCED_FACE('',(#1613),#620,.F.);
#11696=ADVANCED_FACE('',(#1614),#621,.F.);
#11697=ADVANCED_FACE('',(#1615),#622,.F.);
#11698=ADVANCED_FACE('',(#1616),#623,.F.);
#11699=ADVANCED_FACE('',(#1617),#624,.F.);
#11700=ADVANCED_FACE('',(#1618),#625,.F.);
#11701=ADVANCED_FACE('',(#1619,#408),#626,.T.);
#11702=ADVANCED_FACE('',(#1620),#627,.T.);
#11703=ADVANCED_FACE('',(#1621),#628,.T.);
#11704=ADVANCED_FACE('',(#1622),#629,.T.);
#11705=ADVANCED_FACE('',(#1623),#630,.T.);
#11706=ADVANCED_FACE('',(#1624),#631,.T.);
#11707=ADVANCED_FACE('',(#1625),#632,.T.);
#11708=ADVANCED_FACE('',(#1626),#1114,.T.);
#11709=ADVANCED_FACE('',(#1627),#1115,.T.);
#11710=ADVANCED_FACE('',(#1628),#1116,.T.);
#11711=ADVANCED_FACE('',(#1629),#1117,.T.);
#11712=ADVANCED_FACE('',(#1630),#1118,.T.);
#11713=ADVANCED_FACE('',(#1631),#1119,.T.);
#11714=ADVANCED_FACE('',(#1632),#633,.T.);
#11715=ADVANCED_FACE('',(#1633,#409),#634,.T.);
#11716=ADVANCED_FACE('',(#1634),#1120,.T.);
#11717=ADVANCED_FACE('',(#1635),#310,.T.);
#11718=ADVANCED_FACE('',(#1636),#311,.F.);
#11719=ADVANCED_FACE('',(#1637),#312,.F.);
#11720=ADVANCED_FACE('',(#1638),#1121,.T.);
#11721=ADVANCED_FACE('',(#1639),#313,.F.);
#11722=ADVANCED_FACE('',(#1640),#1122,.T.);
#11723=ADVANCED_FACE('',(#1641),#1123,.F.);
#11724=ADVANCED_FACE('',(#1642),#1124,.T.);
#11725=ADVANCED_FACE('',(#1643),#314,.T.);
#11726=ADVANCED_FACE('',(#1644),#315,.F.);
#11727=ADVANCED_FACE('',(#1645),#316,.F.);
#11728=ADVANCED_FACE('',(#1646),#317,.F.);
#11729=ADVANCED_FACE('',(#1647),#1125,.T.);
#11730=ADVANCED_FACE('',(#1648),#1126,.T.);
#11731=ADVANCED_FACE('',(#1649),#1127,.T.);
#11732=ADVANCED_FACE('',(#1650),#1128,.T.);
#11733=ADVANCED_FACE('',(#1651),#1129,.T.);
#11734=ADVANCED_FACE('',(#1652),#1130,.T.);
#11735=ADVANCED_FACE('',(#1653),#1131,.T.);
#11736=ADVANCED_FACE('',(#1654),#11306,.T.);
#11737=ADVANCED_FACE('',(#1655),#1132,.T.);
#11738=ADVANCED_FACE('',(#1656),#1133,.T.);
#11739=ADVANCED_FACE('',(#1657),#11307,.T.);
#11740=ADVANCED_FACE('',(#1658),#1134,.T.);
#11741=ADVANCED_FACE('',(#1659),#1135,.T.);
#11742=ADVANCED_FACE('',(#1660),#635,.F.);
#11743=ADVANCED_FACE('',(#1661),#636,.T.);
#11744=ADVANCED_FACE('',(#1662),#637,.F.);
#11745=ADVANCED_FACE('',(#1663),#638,.T.);
#11746=ADVANCED_FACE('',(#1664),#1136,.T.);
#11747=ADVANCED_FACE('',(#1665),#1137,.T.);
#11748=ADVANCED_FACE('',(#1666),#1138,.T.);
#11749=ADVANCED_FACE('',(#1667),#1139,.T.);
#11750=ADVANCED_FACE('',(#1668),#1140,.T.);
#11751=ADVANCED_FACE('',(#1669),#639,.T.);
#11752=ADVANCED_FACE('',(#1670,#410),#640,.T.);
#11753=ADVANCED_FACE('',(#1671,#411),#641,.T.);
#11754=ADVANCED_FACE('',(#1672,#412),#642,.T.);
#11755=ADVANCED_FACE('',(#1673,#413),#643,.T.);
#11756=ADVANCED_FACE('',(#1674),#644,.T.);
#11757=ADVANCED_FACE('',(#1675),#831,.T.);
#11758=ADVANCED_FACE('',(#1676),#645,.F.);
#11759=ADVANCED_FACE('',(#1677),#646,.T.);
#11760=ADVANCED_FACE('',(#1678),#647,.T.);
#11761=ADVANCED_FACE('',(#1679),#648,.F.);
#11762=ADVANCED_FACE('',(#1680),#1141,.T.);
#11763=ADVANCED_FACE('',(#1681),#649,.F.);
#11764=ADVANCED_FACE('',(#1682),#1142,.T.);
#11765=ADVANCED_FACE('',(#1683),#650,.F.);
#11766=ADVANCED_FACE('',(#1684),#1143,.T.);
#11767=ADVANCED_FACE('',(#1685),#651,.F.);
#11768=ADVANCED_FACE('',(#1686),#1144,.T.);
#11769=ADVANCED_FACE('',(#1687),#652,.F.);
#11770=ADVANCED_FACE('',(#1688),#1145,.F.);
#11771=ADVANCED_FACE('',(#1689),#653,.T.);
#11772=ADVANCED_FACE('',(#1690),#1146,.F.);
#11773=ADVANCED_FACE('',(#1691),#654,.T.);
#11774=ADVANCED_FACE('',(#1692),#1147,.F.);
#11775=ADVANCED_FACE('',(#1693),#655,.T.);
#11776=ADVANCED_FACE('',(#1694),#1148,.F.);
#11777=ADVANCED_FACE('',(#1695),#656,.T.);
#11778=ADVANCED_FACE('',(#1696),#657,.F.);
#11779=ADVANCED_FACE('',(#1697),#1149,.F.);
#11780=ADVANCED_FACE('',(#1698),#658,.F.);
#11781=ADVANCED_FACE('',(#1699),#659,.F.);
#11782=ADVANCED_FACE('',(#1700),#1150,.F.);
#11783=ADVANCED_FACE('',(#1701),#660,.F.);
#11784=ADVANCED_FACE('',(#1702),#661,.F.);
#11785=ADVANCED_FACE('',(#1703),#662,.F.);
#11786=ADVANCED_FACE('',(#1704),#663,.T.);
#11787=ADVANCED_FACE('',(#1705),#664,.T.);
#11788=ADVANCED_FACE('',(#1706),#11,.T.);
#11789=ADVANCED_FACE('',(#1707),#12,.T.);
#11790=ADVANCED_FACE('',(#1708),#1151,.F.);
#11791=ADVANCED_FACE('',(#1709),#11308,.T.);
#11792=ADVANCED_FACE('',(#1710),#1152,.T.);
#11793=ADVANCED_FACE('',(#1711),#832,.F.);
#11794=ADVANCED_FACE('',(#1712),#1153,.T.);
#11795=ADVANCED_FACE('',(#1713),#11309,.T.);
#11796=ADVANCED_FACE('',(#1714),#665,.T.);
#11797=ADVANCED_FACE('',(#1715,#414),#666,.T.);
#11798=ADVANCED_FACE('',(#1716),#667,.T.);
#11799=ADVANCED_FACE('',(#1717),#13,.T.);
#11800=ADVANCED_FACE('',(#1718),#14,.T.);
#11801=ADVANCED_FACE('',(#1719),#15,.T.);
#11802=ADVANCED_FACE('',(#1720),#16,.T.);
#11803=ADVANCED_FACE('',(#1721),#1154,.F.);
#11804=ADVANCED_FACE('',(#1722),#11310,.T.);
#11805=ADVANCED_FACE('',(#1723),#1155,.T.);
#11806=ADVANCED_FACE('',(#1724),#833,.F.);
#11807=ADVANCED_FACE('',(#1725),#1156,.T.);
#11808=ADVANCED_FACE('',(#1726),#11311,.T.);
#11809=ADVANCED_FACE('',(#1727),#668,.T.);
#11810=ADVANCED_FACE('',(#1728,#415),#669,.T.);
#11811=ADVANCED_FACE('',(#1729),#670,.T.);
#11812=ADVANCED_FACE('',(#1730),#17,.T.);
#11813=ADVANCED_FACE('',(#1731),#18,.T.);
#11814=ADVANCED_FACE('',(#1732),#834,.T.);
#11815=ADVANCED_FACE('',(#1733),#835,.T.);
#11816=ADVANCED_FACE('',(#1734),#331,.T.);
#11817=ADVANCED_FACE('',(#1735),#332,.T.);
#11818=ADVANCED_FACE('',(#1736),#1157,.T.);
#11819=ADVANCED_FACE('',(#1737),#1158,.T.);
#11820=ADVANCED_FACE('',(#1738),#1159,.T.);
#11821=ADVANCED_FACE('',(#1739),#1160,.T.);
#11822=ADVANCED_FACE('',(#1740),#1161,.T.);
#11823=ADVANCED_FACE('',(#1741),#318,.F.);
#11824=ADVANCED_FACE('',(#1742),#319,.F.);
#11825=ADVANCED_FACE('',(#1743),#836,.T.);
#11826=ADVANCED_FACE('',(#1744),#837,.T.);
#11827=ADVANCED_FACE('',(#1745),#333,.T.);
#11828=ADVANCED_FACE('',(#1746),#334,.T.);
#11829=ADVANCED_FACE('',(#1747),#1162,.T.);
#11830=ADVANCED_FACE('',(#1748),#1163,.T.);
#11831=ADVANCED_FACE('',(#1749),#1164,.T.);
#11832=ADVANCED_FACE('',(#1750),#1165,.T.);
#11833=ADVANCED_FACE('',(#1751),#1166,.T.);
#11834=ADVANCED_FACE('',(#1752),#320,.F.);
#11835=ADVANCED_FACE('',(#1753),#321,.F.);
#11836=ADVANCED_FACE('',(#1754),#1167,.F.);
#11837=ADVANCED_FACE('',(#1755),#1168,.F.);
#11838=ADVANCED_FACE('',(#1756),#1169,.F.);
#11839=ADVANCED_FACE('',(#1757),#1170,.F.);
#11840=ADVANCED_FACE('',(#1758),#1171,.F.);
#11841=ADVANCED_FACE('',(#1759),#1172,.T.);
#11842=ADVANCED_FACE('',(#1760),#671,.T.);
#11843=ADVANCED_FACE('',(#1761),#672,.F.);
#11844=ADVANCED_FACE('',(#1762),#673,.T.);
#11845=ADVANCED_FACE('',(#1763,#416),#674,.T.);
#11846=ADVANCED_FACE('',(#1764),#675,.F.);
#11847=ADVANCED_FACE('',(#1765),#676,.F.);
#11848=ADVANCED_FACE('',(#1766),#677,.F.);
#11849=ADVANCED_FACE('',(#1767),#678,.T.);
#11850=ADVANCED_FACE('',(#1768,#417,#418),#679,.T.);
#11851=ADVANCED_FACE('',(#1769,#419,#420),#680,.F.);
#11852=ADVANCED_FACE('',(#1770),#681,.T.);
#11853=ADVANCED_FACE('',(#1771),#682,.T.);
#11854=ADVANCED_FACE('',(#1772),#683,.F.);
#11855=ADVANCED_FACE('',(#1773),#684,.T.);
#11856=ADVANCED_FACE('',(#1774,#421,#422),#685,.T.);
#11857=ADVANCED_FACE('',(#1775,#423,#424),#686,.F.);
#11858=ADVANCED_FACE('',(#1776),#1173,.F.);
#11859=ADVANCED_FACE('',(#1777),#1174,.T.);
#11860=ADVANCED_FACE('',(#1778),#687,.F.);
#11861=ADVANCED_FACE('',(#1779),#688,.T.);
#11862=ADVANCED_FACE('',(#1780),#838,.T.);
#11863=ADVANCED_FACE('',(#1781),#322,.F.);
#11864=ADVANCED_FACE('',(#1782),#839,.T.);
#11865=ADVANCED_FACE('',(#1783),#1175,.F.);
#11866=ADVANCED_FACE('',(#1784),#1176,.T.);
#11867=ADVANCED_FACE('',(#1785,#425),#689,.F.);
#11868=ADVANCED_FACE('',(#1786),#840,.T.);
#11869=ADVANCED_FACE('',(#1787),#841,.T.);
#11870=ADVANCED_FACE('',(#1788),#1177,.T.);
#11871=ADVANCED_FACE('',(#1789),#1178,.F.);
#11872=ADVANCED_FACE('',(#1790),#690,.T.);
#11873=ADVANCED_FACE('',(#1791,#426),#691,.F.);
#11874=ADVANCED_FACE('',(#1792),#692,.F.);
#11875=ADVANCED_FACE('',(#1793),#11312,.T.);
#11876=ADVANCED_FACE('',(#1794),#11313,.T.);
#11877=ADVANCED_FACE('',(#1795),#1179,.T.);
#11878=ADVANCED_FACE('',(#1796),#693,.T.);
#11879=ADVANCED_FACE('',(#1797),#694,.F.);
#11880=ADVANCED_FACE('',(#1798),#11314,.F.);
#11881=ADVANCED_FACE('',(#1799),#11315,.F.);
#11882=ADVANCED_FACE('',(#1800),#842,.T.);
#11883=ADVANCED_FACE('',(#1801),#843,.F.);
#11884=ADVANCED_FACE('',(#1802),#844,.T.);
#11885=ADVANCED_FACE('',(#1803),#845,.F.);
#11886=ADVANCED_FACE('',(#1804),#1180,.F.);
#11887=ADVANCED_FACE('',(#1805),#11316,.T.);
#11888=ADVANCED_FACE('',(#1806),#1181,.F.);
#11889=ADVANCED_FACE('',(#1807),#11317,.T.);
#11890=ADVANCED_FACE('',(#1808),#1182,.F.);
#11891=ADVANCED_FACE('',(#1809),#1183,.T.);
#11892=ADVANCED_FACE('',(#1810,#427),#695,.T.);
#11893=ADVANCED_FACE('',(#1811,#428),#696,.F.);
#11894=ADVANCED_FACE('',(#1812,#429),#697,.T.);
#11895=ADVANCED_FACE('',(#1813,#430),#698,.T.);
#11896=ADVANCED_FACE('',(#1814,#431),#699,.F.);
#11897=ADVANCED_FACE('',(#1815,#432),#700,.T.);
#11898=ADVANCED_FACE('',(#1816),#11318,.F.);
#11899=ADVANCED_FACE('',(#1817),#11319,.F.);
#11900=ADVANCED_FACE('',(#1818),#846,.T.);
#11901=ADVANCED_FACE('',(#1819),#847,.F.);
#11902=ADVANCED_FACE('',(#1820),#848,.T.);
#11903=ADVANCED_FACE('',(#1821),#849,.F.);
#11904=ADVANCED_FACE('',(#1822),#1184,.F.);
#11905=ADVANCED_FACE('',(#1823),#11320,.T.);
#11906=ADVANCED_FACE('',(#1824),#1185,.F.);
#11907=ADVANCED_FACE('',(#1825),#11321,.T.);
#11908=ADVANCED_FACE('',(#1826),#1186,.F.);
#11909=ADVANCED_FACE('',(#1827),#1187,.T.);
#11910=ADVANCED_FACE('',(#1828,#433),#701,.T.);
#11911=ADVANCED_FACE('',(#1829,#434),#702,.F.);
#11912=ADVANCED_FACE('',(#1830,#435),#703,.T.);
#11913=ADVANCED_FACE('',(#1831,#436),#704,.T.);
#11914=ADVANCED_FACE('',(#1832,#437),#705,.F.);
#11915=ADVANCED_FACE('',(#1833,#438),#706,.T.);
#11916=ADVANCED_FACE('',(#1834),#11322,.T.);
#11917=ADVANCED_FACE('',(#1835),#11323,.T.);
#11918=ADVANCED_FACE('',(#1836),#1188,.T.);
#11919=ADVANCED_FACE('',(#1837),#707,.T.);
#11920=ADVANCED_FACE('',(#1838),#708,.T.);
#11921=ADVANCED_FACE('',(#1839),#1189,.T.);
#11922=ADVANCED_FACE('',(#1840),#1190,.T.);
#11923=ADVANCED_FACE('',(#1841),#1191,.T.);
#11924=ADVANCED_FACE('',(#1842),#1192,.T.);
#11925=ADVANCED_FACE('',(#1843),#1193,.T.);
#11926=ADVANCED_FACE('',(#1844),#1194,.T.);
#11927=ADVANCED_FACE('',(#1845),#1195,.T.);
#11928=ADVANCED_FACE('',(#1846),#1196,.T.);
#11929=ADVANCED_FACE('',(#1847),#1197,.T.);
#11930=ADVANCED_FACE('',(#1848),#1198,.T.);
#11931=ADVANCED_FACE('',(#1849),#1199,.T.);
#11932=ADVANCED_FACE('',(#1850),#1200,.T.);
#11933=ADVANCED_FACE('',(#1851),#1201,.T.);
#11934=ADVANCED_FACE('',(#1852),#1202,.T.);
#11935=ADVANCED_FACE('',(#1853),#1203,.T.);
#11936=ADVANCED_FACE('',(#1854),#1204,.T.);
#11937=ADVANCED_FACE('',(#1855),#1205,.T.);
#11938=ADVANCED_FACE('',(#1856),#1206,.T.);
#11939=ADVANCED_FACE('',(#1857),#1207,.T.);
#11940=ADVANCED_FACE('',(#1858),#1208,.T.);
#11941=ADVANCED_FACE('',(#1859),#1209,.T.);
#11942=ADVANCED_FACE('',(#1860),#1210,.T.);
#11943=ADVANCED_FACE('',(#1861),#1211,.T.);
#11944=ADVANCED_FACE('',(#1862),#1212,.T.);
#11945=ADVANCED_FACE('',(#1863),#1213,.T.);
#11946=ADVANCED_FACE('',(#1864),#1214,.T.);
#11947=ADVANCED_FACE('',(#1865),#1215,.T.);
#11948=ADVANCED_FACE('',(#1866),#1216,.F.);
#11949=ADVANCED_FACE('',(#1867),#1217,.F.);
#11950=ADVANCED_FACE('',(#1868),#11324,.T.);
#11951=ADVANCED_FACE('',(#1869),#709,.T.);
#11952=ADVANCED_FACE('',(#1870),#710,.T.);
#11953=ADVANCED_FACE('',(#1871,#439),#711,.T.);
#11954=ADVANCED_FACE('',(#1872,#440),#712,.T.);
#11955=ADVANCED_FACE('',(#1873),#713,.T.);
#11956=ADVANCED_FACE('',(#1874,#441),#714,.T.);
#11957=ADVANCED_FACE('',(#1875,#442),#715,.T.);
#11958=ADVANCED_FACE('',(#1876),#716,.T.);
#11959=ADVANCED_FACE('',(#1877),#717,.T.);
#11960=ADVANCED_FACE('',(#1878),#718,.F.);
#11961=ADVANCED_FACE('',(#1879),#719,.F.);
#11962=ADVANCED_FACE('',(#1880),#720,.F.);
#11963=ADVANCED_FACE('',(#1881),#1218,.T.);
#11964=ADVANCED_FACE('',(#1882),#1219,.T.);
#11965=ADVANCED_FACE('',(#1883),#721,.F.);
#11966=ADVANCED_FACE('',(#1884),#722,.F.);
#11967=ADVANCED_FACE('',(#1885,#443),#723,.T.);
#11968=ADVANCED_FACE('',(#1886),#724,.T.);
#11969=ADVANCED_FACE('',(#1887),#725,.F.);
#11970=ADVANCED_FACE('',(#1888),#323,.T.);
#11971=ADVANCED_FACE('',(#1889),#1220,.T.);
#11972=ADVANCED_FACE('',(#1890),#324,.T.);
#11973=ADVANCED_FACE('',(#1891),#1221,.T.);
#11974=ADVANCED_FACE('',(#1892),#1222,.T.);
#11975=ADVANCED_FACE('',(#1893),#1223,.F.);
#11976=ADVANCED_FACE('',(#1894),#1224,.F.);
#11977=ADVANCED_FACE('',(#1895),#1225,.F.);
#11978=ADVANCED_FACE('',(#1896),#1226,.F.);
#11979=ADVANCED_FACE('',(#1897),#1227,.F.);
#11980=ADVANCED_FACE('',(#1898),#1228,.F.);
#11981=ADVANCED_FACE('',(#1899),#1229,.F.);
#11982=ADVANCED_FACE('',(#1900),#1230,.F.);
#11983=ADVANCED_FACE('',(#1901),#1231,.F.);
#11984=ADVANCED_FACE('',(#1902),#1232,.F.);
#11985=ADVANCED_FACE('',(#1903),#1233,.F.);
#11986=ADVANCED_FACE('',(#1904),#1234,.F.);
#11987=ADVANCED_FACE('',(#1905),#1235,.F.);
#11988=ADVANCED_FACE('',(#1906),#1236,.F.);
#11989=ADVANCED_FACE('',(#1907),#1237,.F.);
#11990=ADVANCED_FACE('',(#1908),#1238,.F.);
#11991=ADVANCED_FACE('',(#1909),#1239,.F.);
#11992=ADVANCED_FACE('',(#1910),#1240,.F.);
#11993=ADVANCED_FACE('',(#1911),#1241,.F.);
#11994=ADVANCED_FACE('',(#1912),#1242,.T.);
#11995=ADVANCED_FACE('',(#1913,#444),#726,.T.);
#11996=ADVANCED_FACE('',(#1914,#445),#727,.T.);
#11997=ADVANCED_FACE('',(#1915,#446),#728,.F.);
#11998=ADVANCED_FACE('',(#1916),#729,.F.);
#11999=ADVANCED_FACE('',(#1917),#730,.F.);
#12000=ADVANCED_FACE('',(#1918),#731,.F.);
#12001=ADVANCED_FACE('',(#1919),#732,.F.);
#12002=ADVANCED_FACE('',(#1920),#733,.F.);
#12003=ADVANCED_FACE('',(#1921),#734,.F.);
#12004=ADVANCED_FACE('',(#1922),#735,.F.);
#12005=ADVANCED_FACE('',(#1923),#1243,.F.);
#12006=ADVANCED_FACE('',(#1924),#325,.T.);
#12007=ADVANCED_FACE('',(#1925),#326,.T.);
#12008=ADVANCED_FACE('',(#1926),#736,.T.);
#12009=ADVANCED_FACE('',(#1927),#737,.T.);
#12010=ADVANCED_FACE('',(#1928),#738,.T.);
#12011=ADVANCED_FACE('',(#1929),#739,.T.);
#12012=ADVANCED_FACE('',(#1930),#740,.T.);
#12013=ADVANCED_FACE('',(#1931),#741,.T.);
#12014=ADVANCED_FACE('',(#1932),#11325,.T.);
#12015=ADVANCED_FACE('',(#1933),#11326,.T.);
#12016=ADVANCED_FACE('',(#1934),#1244,.T.);
#12017=ADVANCED_FACE('',(#1935),#1245,.T.);
#12018=ADVANCED_FACE('',(#1936),#742,.F.);
#12019=ADVANCED_FACE('',(#1937),#743,.T.);
#12020=ADVANCED_FACE('',(#1938,#447),#744,.F.);
#12021=ADVANCED_FACE('',(#1939),#11327,.T.);
#12022=ADVANCED_FACE('',(#1940),#11328,.T.);
#12023=ADVANCED_FACE('',(#1941),#1246,.T.);
#12024=ADVANCED_FACE('',(#1942),#745,.T.);
#12025=ADVANCED_FACE('',(#1943),#746,.F.);
#12026=CLOSED_SHELL('',(#11329,#11330,#11331,#11332,#11333,#11334,#11335,
#11336,#11337,#11338,#11339,#11340,#11341,#11342,#11343,#11344,#11345,#11346,
#11347,#11348,#11349,#11350,#11351,#11352,#11353,#11354,#11355,#11356,#11357,
#11358,#11359,#11360,#11361,#11362,#11363,#11364,#11365,#11366,#11367,#11368,
#11369,#11370,#11371,#11372,#11373,#11374,#11375,#11376,#11377,#11378,#11379,
#11380,#11381,#11382,#11383,#11384,#11385,#11386,#11387,#11388,#11389,#11390,
#11391,#11392,#11393,#11394,#11395,#11396,#11397,#11398,#11399,#11400,#11401,
#11402,#11403,#11404,#11405,#11406,#11407,#11408,#11409,#11410,#11411,#11412,
#11413,#11414,#11415,#11416,#11417,#11418,#11419,#11420,#11421,#11422,#11423,
#11424,#11425,#11426,#11427,#11428,#11429,#11430,#11431,#11432,#11433,#11434,
#11435,#11436,#11437,#11438,#11439,#11440,#11441,#11442,#11443,#11444,#11445,
#11446,#11447,#11448,#11449,#11450,#11451,#11452,#11453,#11454,#11455,#11456,
#11457,#11458,#11459,#11460,#11461,#11462,#11463,#11464,#11465,#11466,#11467,
#11468,#11469,#11470,#11471,#11472,#11473,#11474,#11475,#11476,#11477,#11478,
#11479,#11480,#11481,#11482,#11483,#11484,#11485,#11486,#11487,#11488,#11489,
#11490,#11491));
#12027=CLOSED_SHELL('',(#11492,#11493,#11494,#11495,#11496,#11497,#11498,
#11499,#11500,#11501,#11502,#11503,#11504,#11505,#11506,#11507,#11508,#11509,
#11510,#11511,#11512,#11513,#11514,#11515,#11516,#11517,#11518,#11519,#11520,
#11521,#11522,#11523,#11524,#11525,#11526,#11527,#11528,#11529,#11530,#11531,
#11532,#11533,#11534,#11535,#11536,#11537));
#12028=CLOSED_SHELL('',(#11538,#11539,#11540,#11541,#11542,#11543,#11544,
#11545));
#12029=CLOSED_SHELL('',(#11546,#11547,#11548,#11549,#11550,#11551,#11552,
#11553));
#12030=CLOSED_SHELL('',(#11554,#11555,#11556,#11557,#11558,#11559,#11560,
#11561,#11562,#11563,#11564,#11565,#11566,#11567,#11568,#11569,#11570,#11571,
#11572,#11573,#11574,#11575,#11576,#11577,#11578,#11579,#11580,#11581,#11582));
#12031=CLOSED_SHELL('',(#11583,#11584,#11585,#11586,#11587,#11588,#11589,
#11590,#11591,#11592,#11593,#11594,#11595,#11596,#11597,#11598,#11599,#11600,
#11601,#11602,#11603,#11604,#11605,#11606,#11607,#11608,#11609,#11610,#11611,
#11612,#11613,#11614,#11615,#11616,#11617,#11618,#11619,#11620,#11621,#11622));
#12032=CLOSED_SHELL('',(#11623,#11624,#11625,#11626,#11627));
#12033=CLOSED_SHELL('',(#11628,#11629,#11630,#11631,#11632));
#12034=CLOSED_SHELL('',(#11633,#11634,#11635,#11636,#11637,#11638,#11639,
#11640,#11641,#11642,#11643,#11644));
#12035=CLOSED_SHELL('',(#11645,#11646,#11647,#11648,#11649,#11650,#11651,
#11652,#11653,#11654,#11655,#11656,#11657,#11658,#11659,#11660,#11661,#11662,
#11663,#11664,#11665,#11666,#11667,#11668,#11669,#11670,#11671,#11672,#11673,
#11674,#11675,#11676,#11677,#11678,#11679,#11680,#11681,#11682,#11683,#11684,
#11685,#11686,#11687,#11688,#11689,#11690,#11691,#11692,#11693,#11694,#11695,
#11696,#11697,#11698,#11699,#11700,#11701,#11702,#11703,#11704,#11705,#11706,
#11707,#11708,#11709,#11710,#11711,#11712,#11713,#11714,#11715,#11716,#11717,
#11718,#11719,#11720,#11721,#11722,#11723,#11724,#11725,#11726,#11727,#11728,
#11729,#11730,#11731,#11732,#11733,#11734,#11735));
#12036=CLOSED_SHELL('',(#11736,#11737,#11738,#11739,#11740,#11741,#11742,
#11743,#11744,#11745));
#12037=CLOSED_SHELL('',(#11746,#11747,#11748,#11749,#11750,#11751,#11752,
#11753,#11754,#11755,#11756));
#12038=CLOSED_SHELL('',(#11757));
#12039=CLOSED_SHELL('',(#11758,#11759,#11760,#11761,#11762,#11763,#11764,
#11765,#11766,#11767,#11768,#11769,#11770,#11771,#11772,#11773,#11774,#11775,
#11776,#11777,#11778,#11779,#11780,#11781,#11782,#11783,#11784,#11785,#11786,
#11787));
#12040=CLOSED_SHELL('',(#11788,#11789,#11790,#11791,#11792,#11793,#11794,
#11795,#11796,#11797,#11798,#11799,#11800));
#12041=CLOSED_SHELL('',(#11801,#11802,#11803,#11804,#11805,#11806,#11807,
#11808,#11809,#11810,#11811,#11812,#11813));
#12042=CLOSED_SHELL('',(#11814,#11815,#11816,#11817,#11818,#11819,#11820,
#11821,#11822,#11823,#11824));
#12043=CLOSED_SHELL('',(#11825,#11826,#11827,#11828,#11829,#11830,#11831,
#11832,#11833,#11834,#11835));
#12044=CLOSED_SHELL('',(#11836,#11837,#11838,#11839,#11840,#11841,#11842,
#11843,#11844,#11845,#11846,#11847,#11848,#11849,#11850,#11851,#11852,#11853,
#11854,#11855,#11856,#11857,#11858,#11859,#11860,#11861,#11862,#11863));
#12045=CLOSED_SHELL('',(#11864,#11865,#11866,#11867));
#12046=CLOSED_SHELL('',(#11868,#11869,#11870,#11871,#11872,#11873,#11874));
#12047=CLOSED_SHELL('',(#11875,#11876,#11877,#11878,#11879));
#12048=CLOSED_SHELL('',(#11880,#11881,#11882,#11883,#11884,#11885,#11886,
#11887,#11888,#11889,#11890,#11891,#11892,#11893,#11894,#11895,#11896,#11897));
#12049=CLOSED_SHELL('',(#11898,#11899,#11900,#11901,#11902,#11903,#11904,
#11905,#11906,#11907,#11908,#11909,#11910,#11911,#11912,#11913,#11914,#11915));
#12050=CLOSED_SHELL('',(#11916,#11917,#11918,#11919,#11920));
#12051=CLOSED_SHELL('',(#11921,#11922,#11923,#11924,#11925,#11926,#11927,
#11928,#11929,#11930,#11931,#11932,#11933,#11934,#11935,#11936,#11937,#11938,
#11939,#11940,#11941,#11942,#11943,#11944,#11945,#11946,#11947,#11948,#11949,
#11950,#11951,#11952,#11953,#11954,#11955,#11956,#11957,#11958,#11959,#11960,
#11961,#11962,#11963,#11964,#11965,#11966,#11967,#11968,#11969,#11970,#11971,
#11972,#11973,#11974,#11975,#11976));
#12052=CLOSED_SHELL('',(#11977,#11978,#11979,#11980,#11981,#11982,#11983,
#11984,#11985,#11986,#11987,#11988,#11989,#11990,#11991,#11992,#11993,#11994,
#11995,#11996,#11997,#11998,#11999,#12000,#12001,#12002,#12003,#12004,#12005,
#12006,#12007,#12008,#12009,#12010,#12011,#12012,#12013));
#12053=CLOSED_SHELL('',(#12014,#12015,#12016,#12017,#12018,#12019,#12020));
#12054=CLOSED_SHELL('',(#12021,#12022,#12023,#12024,#12025));
#12055=DERIVED_UNIT_ELEMENT(#12099,1.);
#12056=DERIVED_UNIT_ELEMENT(#27809,-3.);
#12057=DERIVED_UNIT_ELEMENT(#12099,1.);
#12058=DERIVED_UNIT_ELEMENT(#27809,-3.);
#12059=DERIVED_UNIT_ELEMENT(#12099,1.);
#12060=DERIVED_UNIT_ELEMENT(#27809,-3.);
#12061=DERIVED_UNIT_ELEMENT(#12099,1.);
#12062=DERIVED_UNIT_ELEMENT(#27809,-3.);
#12063=DERIVED_UNIT_ELEMENT(#12099,1.);
#12064=DERIVED_UNIT_ELEMENT(#27809,-3.);
#12065=DERIVED_UNIT_ELEMENT(#12099,1.);
#12066=DERIVED_UNIT_ELEMENT(#27809,-3.);
#12067=DERIVED_UNIT_ELEMENT(#12099,1.);
#12068=DERIVED_UNIT_ELEMENT(#27809,-3.);
#12069=DERIVED_UNIT_ELEMENT(#12099,1.);
#12070=DERIVED_UNIT_ELEMENT(#27809,-3.);
#12071=DERIVED_UNIT_ELEMENT(#12099,1.);
#12072=DERIVED_UNIT_ELEMENT(#27809,-3.);
#12073=DERIVED_UNIT_ELEMENT(#12099,1.);
#12074=DERIVED_UNIT_ELEMENT(#27809,-3.);
#12075=DERIVED_UNIT_ELEMENT(#12099,1.);
#12076=DERIVED_UNIT_ELEMENT(#27809,-3.);
#12077=DERIVED_UNIT_ELEMENT(#12099,1.);
#12078=DERIVED_UNIT_ELEMENT(#27809,-3.);
#12079=DERIVED_UNIT_ELEMENT(#12099,1.);
#12080=DERIVED_UNIT_ELEMENT(#27809,-3.);
#12081=DERIVED_UNIT_ELEMENT(#12099,1.);
#12082=DERIVED_UNIT_ELEMENT(#27809,-3.);
#12083=DERIVED_UNIT_ELEMENT(#12099,1.);
#12084=DERIVED_UNIT_ELEMENT(#27809,-3.);
#12085=DERIVED_UNIT_ELEMENT(#12099,1.);
#12086=DERIVED_UNIT_ELEMENT(#27809,-3.);
#12087=DERIVED_UNIT_ELEMENT(#12099,1.);
#12088=DERIVED_UNIT_ELEMENT(#27809,-3.);
#12089=DERIVED_UNIT_ELEMENT(#12099,1.);
#12090=DERIVED_UNIT_ELEMENT(#27809,-3.);
#12091=DERIVED_UNIT_ELEMENT(#12099,1.);
#12092=DERIVED_UNIT_ELEMENT(#27809,-3.);
#12093=DERIVED_UNIT_ELEMENT(#12099,1.);
#12094=DERIVED_UNIT_ELEMENT(#27809,-3.);
#12095=DERIVED_UNIT_ELEMENT(#12099,1.);
#12096=DERIVED_UNIT_ELEMENT(#27809,-3.);
#12097=DERIVED_UNIT_ELEMENT(#12099,1.);
#12098=DERIVED_UNIT_ELEMENT(#27809,-3.);
#12099=(
MASS_UNIT()
NAMED_UNIT(*)
SI_UNIT(.KILO.,.GRAM.)
);
#12100=DERIVED_UNIT((#12055,#12056));
#12101=DERIVED_UNIT((#12057,#12058));
#12102=DERIVED_UNIT((#12059,#12060));
#12103=DERIVED_UNIT((#12061,#12062));
#12104=DERIVED_UNIT((#12063,#12064));
#12105=DERIVED_UNIT((#12065,#12066));
#12106=DERIVED_UNIT((#12067,#12068));
#12107=DERIVED_UNIT((#12069,#12070));
#12108=DERIVED_UNIT((#12071,#12072));
#12109=DERIVED_UNIT((#12073,#12074));
#12110=DERIVED_UNIT((#12075,#12076));
#12111=DERIVED_UNIT((#12077,#12078));
#12112=DERIVED_UNIT((#12079,#12080));
#12113=DERIVED_UNIT((#12081,#12082));
#12114=DERIVED_UNIT((#12083,#12084));
#12115=DERIVED_UNIT((#12085,#12086));
#12116=DERIVED_UNIT((#12087,#12088));
#12117=DERIVED_UNIT((#12089,#12090));
#12118=DERIVED_UNIT((#12091,#12092));
#12119=DERIVED_UNIT((#12093,#12094));
#12120=DERIVED_UNIT((#12095,#12096));
#12121=DERIVED_UNIT((#12097,#12098));
#12122=MEASURE_REPRESENTATION_ITEM('density measure',
POSITIVE_RATIO_MEASURE(7850.),#12100);
#12123=MEASURE_REPRESENTATION_ITEM('density measure',
POSITIVE_RATIO_MEASURE(7850.),#12101);
#12124=MEASURE_REPRESENTATION_ITEM('density measure',
POSITIVE_RATIO_MEASURE(7850.),#12102);
#12125=MEASURE_REPRESENTATION_ITEM('density measure',
POSITIVE_RATIO_MEASURE(7850.),#12103);
#12126=MEASURE_REPRESENTATION_ITEM('density measure',
POSITIVE_RATIO_MEASURE(7850.),#12104);
#12127=MEASURE_REPRESENTATION_ITEM('density measure',
POSITIVE_RATIO_MEASURE(7850.),#12105);
#12128=MEASURE_REPRESENTATION_ITEM('density measure',
POSITIVE_RATIO_MEASURE(7850.),#12106);
#12129=MEASURE_REPRESENTATION_ITEM('density measure',
POSITIVE_RATIO_MEASURE(7850.),#12107);
#12130=MEASURE_REPRESENTATION_ITEM('density measure',
POSITIVE_RATIO_MEASURE(7850.),#12108);
#12131=MEASURE_REPRESENTATION_ITEM('density measure',
POSITIVE_RATIO_MEASURE(7850.),#12109);
#12132=MEASURE_REPRESENTATION_ITEM('density measure',
POSITIVE_RATIO_MEASURE(7850.),#12110);
#12133=MEASURE_REPRESENTATION_ITEM('density measure',
POSITIVE_RATIO_MEASURE(7850.),#12111);
#12134=MEASURE_REPRESENTATION_ITEM('density measure',
POSITIVE_RATIO_MEASURE(7850.),#12112);
#12135=MEASURE_REPRESENTATION_ITEM('density measure',
POSITIVE_RATIO_MEASURE(7850.),#12113);
#12136=MEASURE_REPRESENTATION_ITEM('density measure',
POSITIVE_RATIO_MEASURE(7850.),#12114);
#12137=MEASURE_REPRESENTATION_ITEM('density measure',
POSITIVE_RATIO_MEASURE(7850.),#12115);
#12138=MEASURE_REPRESENTATION_ITEM('density measure',
POSITIVE_RATIO_MEASURE(7850.),#12116);
#12139=MEASURE_REPRESENTATION_ITEM('density measure',
POSITIVE_RATIO_MEASURE(7850.),#12117);
#12140=MEASURE_REPRESENTATION_ITEM('density measure',
POSITIVE_RATIO_MEASURE(7850.),#12118);
#12141=MEASURE_REPRESENTATION_ITEM('density measure',
POSITIVE_RATIO_MEASURE(7850.),#12119);
#12142=MEASURE_REPRESENTATION_ITEM('density measure',
POSITIVE_RATIO_MEASURE(7850.),#12120);
#12143=MEASURE_REPRESENTATION_ITEM('density measure',
POSITIVE_RATIO_MEASURE(7850.),#12121);
#12144=PROPERTY_DEFINITION_REPRESENTATION(#12254,#12188);
#12145=PROPERTY_DEFINITION_REPRESENTATION(#12255,#12189);
#12146=PROPERTY_DEFINITION_REPRESENTATION(#12256,#12190);
#12147=PROPERTY_DEFINITION_REPRESENTATION(#12257,#12191);
#12148=PROPERTY_DEFINITION_REPRESENTATION(#12258,#12192);
#12149=PROPERTY_DEFINITION_REPRESENTATION(#12259,#12193);
#12150=PROPERTY_DEFINITION_REPRESENTATION(#12260,#12194);
#12151=PROPERTY_DEFINITION_REPRESENTATION(#12261,#12195);
#12152=PROPERTY_DEFINITION_REPRESENTATION(#12262,#12196);
#12153=PROPERTY_DEFINITION_REPRESENTATION(#12263,#12197);
#12154=PROPERTY_DEFINITION_REPRESENTATION(#12264,#12198);
#12155=PROPERTY_DEFINITION_REPRESENTATION(#12265,#12199);
#12156=PROPERTY_DEFINITION_REPRESENTATION(#12266,#12200);
#12157=PROPERTY_DEFINITION_REPRESENTATION(#12267,#12201);
#12158=PROPERTY_DEFINITION_REPRESENTATION(#12268,#12202);
#12159=PROPERTY_DEFINITION_REPRESENTATION(#12269,#12203);
#12160=PROPERTY_DEFINITION_REPRESENTATION(#12270,#12204);
#12161=PROPERTY_DEFINITION_REPRESENTATION(#12271,#12205);
#12162=PROPERTY_DEFINITION_REPRESENTATION(#12272,#12206);
#12163=PROPERTY_DEFINITION_REPRESENTATION(#12273,#12207);
#12164=PROPERTY_DEFINITION_REPRESENTATION(#12274,#12208);
#12165=PROPERTY_DEFINITION_REPRESENTATION(#12275,#12209);
#12166=PROPERTY_DEFINITION_REPRESENTATION(#12276,#12210);
#12167=PROPERTY_DEFINITION_REPRESENTATION(#12277,#12211);
#12168=PROPERTY_DEFINITION_REPRESENTATION(#12278,#12212);
#12169=PROPERTY_DEFINITION_REPRESENTATION(#12279,#12213);
#12170=PROPERTY_DEFINITION_REPRESENTATION(#12280,#12214);
#12171=PROPERTY_DEFINITION_REPRESENTATION(#12281,#12215);
#12172=PROPERTY_DEFINITION_REPRESENTATION(#12282,#12216);
#12173=PROPERTY_DEFINITION_REPRESENTATION(#12283,#12217);
#12174=PROPERTY_DEFINITION_REPRESENTATION(#12284,#12218);
#12175=PROPERTY_DEFINITION_REPRESENTATION(#12285,#12219);
#12176=PROPERTY_DEFINITION_REPRESENTATION(#12286,#12220);
#12177=PROPERTY_DEFINITION_REPRESENTATION(#12287,#12221);
#12178=PROPERTY_DEFINITION_REPRESENTATION(#12288,#12222);
#12179=PROPERTY_DEFINITION_REPRESENTATION(#12289,#12223);
#12180=PROPERTY_DEFINITION_REPRESENTATION(#12290,#12224);
#12181=PROPERTY_DEFINITION_REPRESENTATION(#12291,#12225);
#12182=PROPERTY_DEFINITION_REPRESENTATION(#12292,#12226);
#12183=PROPERTY_DEFINITION_REPRESENTATION(#12293,#12227);
#12184=PROPERTY_DEFINITION_REPRESENTATION(#12294,#12228);
#12185=PROPERTY_DEFINITION_REPRESENTATION(#12295,#12229);
#12186=PROPERTY_DEFINITION_REPRESENTATION(#12296,#12230);
#12187=PROPERTY_DEFINITION_REPRESENTATION(#12297,#12231);
#12188=REPRESENTATION('material name',(#12232),#27780);
#12189=REPRESENTATION('density',(#12122),#27780);
#12190=REPRESENTATION('material name',(#12233),#27782);
#12191=REPRESENTATION('density',(#12123),#27782);
#12192=REPRESENTATION('material name',(#12234),#27783);
#12193=REPRESENTATION('density',(#12124),#27783);
#12194=REPRESENTATION('material name',(#12235),#27785);
#12195=REPRESENTATION('density',(#12125),#27785);
#12196=REPRESENTATION('material name',(#12236),#27786);
#12197=REPRESENTATION('density',(#12126),#27786);
#12198=REPRESENTATION('material name',(#12237),#27787);
#12199=REPRESENTATION('density',(#12127),#27787);
#12200=REPRESENTATION('material name',(#12238),#27788);
#12201=REPRESENTATION('density',(#12128),#27788);
#12202=REPRESENTATION('material name',(#12239),#27790);
#12203=REPRESENTATION('density',(#12129),#27790);
#12204=REPRESENTATION('material name',(#12240),#27791);
#12205=REPRESENTATION('density',(#12130),#27791);
#12206=REPRESENTATION('material name',(#12241),#27792);
#12207=REPRESENTATION('density',(#12131),#27792);
#12208=REPRESENTATION('material name',(#12242),#27793);
#12209=REPRESENTATION('density',(#12132),#27793);
#12210=REPRESENTATION('material name',(#12243),#27794);
#12211=REPRESENTATION('density',(#12133),#27794);
#12212=REPRESENTATION('material name',(#12244),#27795);
#12213=REPRESENTATION('density',(#12134),#27795);
#12214=REPRESENTATION('material name',(#12245),#27796);
#12215=REPRESENTATION('density',(#12135),#27796);
#12216=REPRESENTATION('material name',(#12246),#27798);
#12217=REPRESENTATION('density',(#12136),#27798);
#12218=REPRESENTATION('material name',(#12247),#27799);
#12219=REPRESENTATION('density',(#12137),#27799);
#12220=REPRESENTATION('material name',(#12248),#27800);
#12221=REPRESENTATION('density',(#12138),#27800);
#12222=REPRESENTATION('material name',(#12249),#27802);
#12223=REPRESENTATION('density',(#12139),#27802);
#12224=REPRESENTATION('material name',(#12250),#27803);
#12225=REPRESENTATION('density',(#12140),#27803);
#12226=REPRESENTATION('material name',(#12251),#27804);
#12227=REPRESENTATION('density',(#12141),#27804);
#12228=REPRESENTATION('material name',(#12252),#27805);
#12229=REPRESENTATION('density',(#12142),#27805);
#12230=REPRESENTATION('material name',(#12253),#27806);
#12231=REPRESENTATION('density',(#12143),#27806);
#12232=DESCRIPTIVE_REPRESENTATION_ITEM('Steel','Steel');
#12233=DESCRIPTIVE_REPRESENTATION_ITEM('Steel','Steel');
#12234=DESCRIPTIVE_REPRESENTATION_ITEM('Steel','Steel');
#12235=DESCRIPTIVE_REPRESENTATION_ITEM('Steel','Steel');
#12236=DESCRIPTIVE_REPRESENTATION_ITEM('Steel','Steel');
#12237=DESCRIPTIVE_REPRESENTATION_ITEM('Steel','Steel');
#12238=DESCRIPTIVE_REPRESENTATION_ITEM('Steel','Steel');
#12239=DESCRIPTIVE_REPRESENTATION_ITEM('Steel','Steel');
#12240=DESCRIPTIVE_REPRESENTATION_ITEM('Steel','Steel');
#12241=DESCRIPTIVE_REPRESENTATION_ITEM('Steel','Steel');
#12242=DESCRIPTIVE_REPRESENTATION_ITEM('Steel','Steel');
#12243=DESCRIPTIVE_REPRESENTATION_ITEM('Steel','Steel');
#12244=DESCRIPTIVE_REPRESENTATION_ITEM('Steel','Steel');
#12245=DESCRIPTIVE_REPRESENTATION_ITEM('Steel','Steel');
#12246=DESCRIPTIVE_REPRESENTATION_ITEM('Steel','Steel');
#12247=DESCRIPTIVE_REPRESENTATION_ITEM('Steel','Steel');
#12248=DESCRIPTIVE_REPRESENTATION_ITEM('Steel','Steel');
#12249=DESCRIPTIVE_REPRESENTATION_ITEM('Steel','Steel');
#12250=DESCRIPTIVE_REPRESENTATION_ITEM('Steel','Steel');
#12251=DESCRIPTIVE_REPRESENTATION_ITEM('Steel','Steel');
#12252=DESCRIPTIVE_REPRESENTATION_ITEM('Steel','Steel');
#12253=DESCRIPTIVE_REPRESENTATION_ITEM('Steel','Steel');
#12254=PROPERTY_DEFINITION('material property','material name',#27929);
#12255=PROPERTY_DEFINITION('material property','density of part',#27929);
#12256=PROPERTY_DEFINITION('material property','material name',#27931);
#12257=PROPERTY_DEFINITION('material property','density of part',#27931);
#12258=PROPERTY_DEFINITION('material property','material name',#27932);
#12259=PROPERTY_DEFINITION('material property','density of part',#27932);
#12260=PROPERTY_DEFINITION('material property','material name',#27934);
#12261=PROPERTY_DEFINITION('material property','density of part',#27934);
#12262=PROPERTY_DEFINITION('material property','material name',#27935);
#12263=PROPERTY_DEFINITION('material property','density of part',#27935);
#12264=PROPERTY_DEFINITION('material property','material name',#27936);
#12265=PROPERTY_DEFINITION('material property','density of part',#27936);
#12266=PROPERTY_DEFINITION('material property','material name',#27937);
#12267=PROPERTY_DEFINITION('material property','density of part',#27937);
#12268=PROPERTY_DEFINITION('material property','material name',#27939);
#12269=PROPERTY_DEFINITION('material property','density of part',#27939);
#12270=PROPERTY_DEFINITION('material property','material name',#27940);
#12271=PROPERTY_DEFINITION('material property','density of part',#27940);
#12272=PROPERTY_DEFINITION('material property','material name',#27941);
#12273=PROPERTY_DEFINITION('material property','density of part',#27941);
#12274=PROPERTY_DEFINITION('material property','material name',#27942);
#12275=PROPERTY_DEFINITION('material property','density of part',#27942);
#12276=PROPERTY_DEFINITION('material property','material name',#27943);
#12277=PROPERTY_DEFINITION('material property','density of part',#27943);
#12278=PROPERTY_DEFINITION('material property','material name',#27944);
#12279=PROPERTY_DEFINITION('material property','density of part',#27944);
#12280=PROPERTY_DEFINITION('material property','material name',#27945);
#12281=PROPERTY_DEFINITION('material property','density of part',#27945);
#12282=PROPERTY_DEFINITION('material property','material name',#27947);
#12283=PROPERTY_DEFINITION('material property','density of part',#27947);
#12284=PROPERTY_DEFINITION('material property','material name',#27948);
#12285=PROPERTY_DEFINITION('material property','density of part',#27948);
#12286=PROPERTY_DEFINITION('material property','material name',#27949);
#12287=PROPERTY_DEFINITION('material property','density of part',#27949);
#12288=PROPERTY_DEFINITION('material property','material name',#27951);
#12289=PROPERTY_DEFINITION('material property','density of part',#27951);
#12290=PROPERTY_DEFINITION('material property','material name',#27952);
#12291=PROPERTY_DEFINITION('material property','density of part',#27952);
#12292=PROPERTY_DEFINITION('material property','material name',#27953);
#12293=PROPERTY_DEFINITION('material property','density of part',#27953);
#12294=PROPERTY_DEFINITION('material property','material name',#27954);
#12295=PROPERTY_DEFINITION('material property','density of part',#27954);
#12296=PROPERTY_DEFINITION('material property','material name',#27955);
#12297=PROPERTY_DEFINITION('material property','density of part',#27955);
#12298=AXIS2_PLACEMENT_3D('',#17420,#13732,#13733);
#12299=AXIS2_PLACEMENT_3D('',#17421,#13734,#13735);
#12300=AXIS2_PLACEMENT_3D('',#17422,#13736,#13737);
#12301=AXIS2_PLACEMENT_3D('',#17424,#13738,#13739);
#12302=AXIS2_PLACEMENT_3D('',#17427,#13741,#13742);
#12303=AXIS2_PLACEMENT_3D('',#17428,#13743,#13744);
#12304=AXIS2_PLACEMENT_3D('',#17430,#13745,#13746);
#12305=AXIS2_PLACEMENT_3D('',#17433,#13748,#13749);
#12306=AXIS2_PLACEMENT_3D('',#17434,#13750,#13751);
#12307=AXIS2_PLACEMENT_3D('',#17436,#13752,#13753);
#12308=AXIS2_PLACEMENT_3D('',#17439,#13755,#13756);
#12309=AXIS2_PLACEMENT_3D('',#17440,#13757,#13758);
#12310=AXIS2_PLACEMENT_3D('',#17442,#13759,#13760);
#12311=AXIS2_PLACEMENT_3D('',#17445,#13762,#13763);
#12312=AXIS2_PLACEMENT_3D('',#17446,#13764,#13765);
#12313=AXIS2_PLACEMENT_3D('',#17448,#13766,#13767);
#12314=AXIS2_PLACEMENT_3D('',#17451,#13769,#13770);
#12315=AXIS2_PLACEMENT_3D('',#17452,#13771,#13772);
#12316=AXIS2_PLACEMENT_3D('',#17454,#13773,#13774);
#12317=AXIS2_PLACEMENT_3D('',#17457,#13776,#13777);
#12318=AXIS2_PLACEMENT_3D('',#17458,#13778,#13779);
#12319=AXIS2_PLACEMENT_3D('',#17461,#13780,#13781);
#12320=AXIS2_PLACEMENT_3D('',#17465,#13783,#13784);
#12321=AXIS2_PLACEMENT_3D('',#17480,#13786,#13787);
#12322=AXIS2_PLACEMENT_3D('',#17483,#13788,#13789);
#12323=AXIS2_PLACEMENT_3D('',#17485,#13790,#13791);
#12324=AXIS2_PLACEMENT_3D('',#17487,#13792,#13793);
#12325=AXIS2_PLACEMENT_3D('',#17488,#13794,#13795);
#12326=AXIS2_PLACEMENT_3D('',#17489,#13796,#13797);
#12327=AXIS2_PLACEMENT_3D('',#17491,#13798,#13799);
#12328=AXIS2_PLACEMENT_3D('',#17493,#13800,#13801);
#12329=AXIS2_PLACEMENT_3D('',#17494,#13802,#13803);
#12330=AXIS2_PLACEMENT_3D('',#17495,#13804,#13805);
#12331=AXIS2_PLACEMENT_3D('',#17497,#13806,#13807);
#12332=AXIS2_PLACEMENT_3D('',#17499,#13808,#13809);
#12333=AXIS2_PLACEMENT_3D('',#17500,#13810,#13811);
#12334=AXIS2_PLACEMENT_3D('',#17501,#13812,#13813);
#12335=AXIS2_PLACEMENT_3D('',#17503,#13814,#13815);
#12336=AXIS2_PLACEMENT_3D('',#17505,#13816,#13817);
#12337=AXIS2_PLACEMENT_3D('',#17506,#13818,#13819);
#12338=AXIS2_PLACEMENT_3D('',#17507,#13820,#13821);
#12339=AXIS2_PLACEMENT_3D('',#17509,#13822,#13823);
#12340=AXIS2_PLACEMENT_3D('',#17511,#13824,#13825);
#12341=AXIS2_PLACEMENT_3D('',#17512,#13826,#13827);
#12342=AXIS2_PLACEMENT_3D('',#17513,#13828,#13829);
#12343=AXIS2_PLACEMENT_3D('',#17516,#13830,#13831);
#12344=AXIS2_PLACEMENT_3D('',#17518,#13832,#13833);
#12345=AXIS2_PLACEMENT_3D('',#17520,#13834,#13835);
#12346=AXIS2_PLACEMENT_3D('',#17522,#13836,#13837);
#12347=AXIS2_PLACEMENT_3D('',#17523,#13838,#13839);
#12348=AXIS2_PLACEMENT_3D('',#17524,#13840,#13841);
#12349=AXIS2_PLACEMENT_3D('',#17527,#13842,#13843);
#12350=AXIS2_PLACEMENT_3D('',#17529,#13844,#13845);
#12351=AXIS2_PLACEMENT_3D('',#17531,#13846,#13847);
#12352=AXIS2_PLACEMENT_3D('',#17533,#13848,#13849);
#12353=AXIS2_PLACEMENT_3D('',#17534,#13850,#13851);
#12354=AXIS2_PLACEMENT_3D('',#17535,#13852,#13853);
#12355=AXIS2_PLACEMENT_3D('',#17537,#13854,#13855);
#12356=AXIS2_PLACEMENT_3D('',#17539,#13856,#13857);
#12357=AXIS2_PLACEMENT_3D('',#17541,#13858,#13859);
#12358=AXIS2_PLACEMENT_3D('',#17542,#13860,#13861);
#12359=AXIS2_PLACEMENT_3D('',#17543,#13862,#13863);
#12360=AXIS2_PLACEMENT_3D('',#17545,#13864,#13865);
#12361=AXIS2_PLACEMENT_3D('',#17547,#13866,#13867);
#12362=AXIS2_PLACEMENT_3D('',#17548,#13868,#13869);
#12363=AXIS2_PLACEMENT_3D('',#17549,#13870,#13871);
#12364=AXIS2_PLACEMENT_3D('',#17552,#13872,#13873);
#12365=AXIS2_PLACEMENT_3D('',#17553,#13874,#13875);
#12366=AXIS2_PLACEMENT_3D('',#17555,#13876,#13877);
#12367=AXIS2_PLACEMENT_3D('',#17556,#13878,#13879);
#12368=AXIS2_PLACEMENT_3D('',#17557,#13880,#13881);
#12369=AXIS2_PLACEMENT_3D('',#17560,#13882,#13883);
#12370=AXIS2_PLACEMENT_3D('',#17561,#13884,#13885);
#12371=AXIS2_PLACEMENT_3D('',#17563,#13886,#13887);
#12372=AXIS2_PLACEMENT_3D('',#17564,#13888,#13889);
#12373=AXIS2_PLACEMENT_3D('',#17565,#13890,#13891);
#12374=AXIS2_PLACEMENT_3D('',#17568,#13892,#13893);
#12375=AXIS2_PLACEMENT_3D('',#17572,#13895,#13896);
#12376=AXIS2_PLACEMENT_3D('',#17574,#13897,#13898);
#12377=AXIS2_PLACEMENT_3D('',#17577,#13900,#13901);
#12378=AXIS2_PLACEMENT_3D('',#17578,#13902,#13903);
#12379=AXIS2_PLACEMENT_3D('',#17581,#13904,#13905);
#12380=AXIS2_PLACEMENT_3D('',#17583,#13906,#13907);
#12381=AXIS2_PLACEMENT_3D('',#17585,#13908,#13909);
#12382=AXIS2_PLACEMENT_3D('',#17586,#13910,#13911);
#12383=AXIS2_PLACEMENT_3D('',#17587,#13912,#13913);
#12384=AXIS2_PLACEMENT_3D('',#17589,#13914,#13915);
#12385=AXIS2_PLACEMENT_3D('',#17592,#13917,#13918);
#12386=AXIS2_PLACEMENT_3D('',#17593,#13919,#13920);
#12387=AXIS2_PLACEMENT_3D('',#17595,#13922,#13923);
#12388=AXIS2_PLACEMENT_3D('',#17609,#13925,#13926);
#12389=AXIS2_PLACEMENT_3D('',#17611,#13928,#13929);
#12390=AXIS2_PLACEMENT_3D('',#17615,#13931,#13932);
#12391=AXIS2_PLACEMENT_3D('',#17617,#13934,#13935);
#12392=AXIS2_PLACEMENT_3D('',#17620,#13937,#13938);
#12393=AXIS2_PLACEMENT_3D('',#17621,#13939,#13940);
#12394=AXIS2_PLACEMENT_3D('',#17623,#13941,#13942);
#12395=AXIS2_PLACEMENT_3D('',#17626,#13944,#13945);
#12396=AXIS2_PLACEMENT_3D('',#17627,#13946,#13947);
#12397=AXIS2_PLACEMENT_3D('',#17629,#13948,#13949);
#12398=AXIS2_PLACEMENT_3D('',#17632,#13951,#13952);
#12399=AXIS2_PLACEMENT_3D('',#17633,#13953,#13954);
#12400=AXIS2_PLACEMENT_3D('',#17635,#13955,#13956);
#12401=AXIS2_PLACEMENT_3D('',#17638,#13958,#13959);
#12402=AXIS2_PLACEMENT_3D('',#17639,#13960,#13961);
#12403=AXIS2_PLACEMENT_3D('',#17641,#13963,#13964);
#12404=AXIS2_PLACEMENT_3D('',#17655,#13966,#13967);
#12405=AXIS2_PLACEMENT_3D('',#17657,#13969,#13970);
#12406=AXIS2_PLACEMENT_3D('',#17660,#13972,#13973);
#12407=AXIS2_PLACEMENT_3D('',#17661,#13974,#13975);
#12408=AXIS2_PLACEMENT_3D('',#17663,#13976,#13977);
#12409=AXIS2_PLACEMENT_3D('',#17666,#13979,#13980);
#12410=AXIS2_PLACEMENT_3D('',#17667,#13981,#13982);
#12411=AXIS2_PLACEMENT_3D('',#17669,#13983,#13984);
#12412=AXIS2_PLACEMENT_3D('',#17672,#13986,#13987);
#12413=AXIS2_PLACEMENT_3D('',#17673,#13988,#13989);
#12414=AXIS2_PLACEMENT_3D('',#17675,#13990,#13991);
#12415=AXIS2_PLACEMENT_3D('',#17678,#13993,#13994);
#12416=AXIS2_PLACEMENT_3D('',#17679,#13995,#13996);
#12417=AXIS2_PLACEMENT_3D('',#17681,#13998,#13999);
#12418=AXIS2_PLACEMENT_3D('',#17683,#14000,#14001);
#12419=AXIS2_PLACEMENT_3D('',#17686,#14003,#14004);
#12420=AXIS2_PLACEMENT_3D('',#17687,#14005,#14006);
#12421=AXIS2_PLACEMENT_3D('',#17691,#14008,#14009);
#12422=AXIS2_PLACEMENT_3D('',#17693,#14011,#14012);
#12423=AXIS2_PLACEMENT_3D('',#17695,#14013,#14014);
#12424=AXIS2_PLACEMENT_3D('',#17698,#14016,#14017);
#12425=AXIS2_PLACEMENT_3D('',#17699,#14018,#14019);
#12426=AXIS2_PLACEMENT_3D('',#17708,#14023,#14024);
#12427=AXIS2_PLACEMENT_3D('',#17710,#14026,#14027);
#12428=AXIS2_PLACEMENT_3D('',#17719,#14032,#14033);
#12429=AXIS2_PLACEMENT_3D('',#17727,#14038,#14039);
#12430=AXIS2_PLACEMENT_3D('',#17737,#14044,#14045);
#12431=AXIS2_PLACEMENT_3D('',#17738,#14046,#14047);
#12432=AXIS2_PLACEMENT_3D('',#17747,#14052,#14053);
#12433=AXIS2_PLACEMENT_3D('',#17756,#14057,#14058);
#12434=AXIS2_PLACEMENT_3D('',#17758,#14060,#14061);
#12435=AXIS2_PLACEMENT_3D('',#17761,#14062,#14063);
#12436=AXIS2_PLACEMENT_3D('',#17764,#14065,#14066);
#12437=AXIS2_PLACEMENT_3D('',#17765,#14067,#14068);
#12438=AXIS2_PLACEMENT_3D('',#17767,#14069,#14070);
#12439=AXIS2_PLACEMENT_3D('',#17771,#14072,#14073);
#12440=AXIS2_PLACEMENT_3D('',#17778,#14074,#14075);
#12441=AXIS2_PLACEMENT_3D('',#17787,#14079,#14080);
#12442=AXIS2_PLACEMENT_3D('',#17790,#14082,#14083);
#12443=AXIS2_PLACEMENT_3D('',#17791,#14084,#14085);
#12444=AXIS2_PLACEMENT_3D('',#17800,#14090,#14091);
#12445=AXIS2_PLACEMENT_3D('',#17811,#14098,#14099);
#12446=AXIS2_PLACEMENT_3D('',#17813,#14100,#14101);
#12447=AXIS2_PLACEMENT_3D('',#17816,#14103,#14104);
#12448=AXIS2_PLACEMENT_3D('',#17817,#14105,#14106);
#12449=AXIS2_PLACEMENT_3D('',#17821,#14108,#14109);
#12450=AXIS2_PLACEMENT_3D('',#17822,#14110,#14111);
#12451=AXIS2_PLACEMENT_3D('',#17823,#14112,#14113);
#12452=AXIS2_PLACEMENT_3D('',#17829,#14117,#14118);
#12453=AXIS2_PLACEMENT_3D('',#17835,#14122,#14123);
#12454=AXIS2_PLACEMENT_3D('',#17839,#14126,#14127);
#12455=AXIS2_PLACEMENT_3D('',#17840,#14128,#14129);
#12456=AXIS2_PLACEMENT_3D('',#17844,#14132,#14133);
#12457=AXIS2_PLACEMENT_3D('',#17845,#14134,#14135);
#12458=AXIS2_PLACEMENT_3D('',#17847,#14136,#14137);
#12459=AXIS2_PLACEMENT_3D('',#17850,#14139,#14140);
#12460=AXIS2_PLACEMENT_3D('',#17852,#14141,#14142);
#12461=AXIS2_PLACEMENT_3D('',#17856,#14144,#14145);
#12462=AXIS2_PLACEMENT_3D('',#17864,#14150,#14151);
#12463=AXIS2_PLACEMENT_3D('',#17867,#14153,#14154);
#12464=AXIS2_PLACEMENT_3D('',#17871,#14156,#14157);
#12465=AXIS2_PLACEMENT_3D('',#17873,#14159,#14160);
#12466=AXIS2_PLACEMENT_3D('',#17874,#14161,#14162);
#12467=AXIS2_PLACEMENT_3D('',#17879,#14164,#14165);
#12468=AXIS2_PLACEMENT_3D('',#17882,#14167,#14168);
#12469=AXIS2_PLACEMENT_3D('',#17884,#14169,#14170);
#12470=AXIS2_PLACEMENT_3D('',#17888,#14172,#14173);
#12471=AXIS2_PLACEMENT_3D('',#17892,#14175,#14176);
#12472=AXIS2_PLACEMENT_3D('',#17896,#14178,#14179);
#12473=AXIS2_PLACEMENT_3D('',#17897,#14180,#14181);
#12474=AXIS2_PLACEMENT_3D('',#17899,#14182,#14183);
#12475=AXIS2_PLACEMENT_3D('',#17903,#14185,#14186);
#12476=AXIS2_PLACEMENT_3D('',#17906,#14188,#14189);
#12477=AXIS2_PLACEMENT_3D('',#17907,#14190,#14191);
#12478=AXIS2_PLACEMENT_3D('',#17913,#14195,#14196);
#12479=AXIS2_PLACEMENT_3D('',#17922,#14201,#14202);
#12480=AXIS2_PLACEMENT_3D('',#17924,#14203,#14204);
#12481=AXIS2_PLACEMENT_3D('',#17927,#14206,#14207);
#12482=AXIS2_PLACEMENT_3D('',#17928,#14208,#14209);
#12483=AXIS2_PLACEMENT_3D('',#17930,#14210,#14211);
#12484=AXIS2_PLACEMENT_3D('',#17934,#14213,#14214);
#12485=AXIS2_PLACEMENT_3D('',#17938,#14216,#14217);
#12486=AXIS2_PLACEMENT_3D('',#17942,#14219,#14220);
#12487=AXIS2_PLACEMENT_3D('',#17946,#14222,#14223);
#12488=AXIS2_PLACEMENT_3D('',#17951,#14226,#14227);
#12489=AXIS2_PLACEMENT_3D('',#17953,#14228,#14229);
#12490=AXIS2_PLACEMENT_3D('',#17956,#14231,#14232);
#12491=AXIS2_PLACEMENT_3D('',#17960,#14234,#14235);
#12492=AXIS2_PLACEMENT_3D('',#17964,#14237,#14238);
#12493=AXIS2_PLACEMENT_3D('',#17967,#14241,#14242);
#12494=AXIS2_PLACEMENT_3D('',#17970,#14245,#14246);
#12495=AXIS2_PLACEMENT_3D('',#17973,#14249,#14250);
#12496=AXIS2_PLACEMENT_3D('',#17976,#14253,#14254);
#12497=AXIS2_PLACEMENT_3D('',#17979,#14257,#14258);
#12498=AXIS2_PLACEMENT_3D('',#17980,#14259,#14260);
#12499=AXIS2_PLACEMENT_3D('',#17985,#14263,#14264);
#12500=AXIS2_PLACEMENT_3D('',#17987,#14266,#14267);
#12501=AXIS2_PLACEMENT_3D('',#17991,#14269,#14270);
#12502=AXIS2_PLACEMENT_3D('',#17992,#14271,#14272);
#12503=AXIS2_PLACEMENT_3D('',#17993,#14273,#14274);
#12504=AXIS2_PLACEMENT_3D('',#17998,#14277,#14278);
#12505=AXIS2_PLACEMENT_3D('',#18001,#14280,#14281);
#12506=AXIS2_PLACEMENT_3D('',#18002,#14282,#14283);
#12507=AXIS2_PLACEMENT_3D('',#18005,#14284,#14285);
#12508=AXIS2_PLACEMENT_3D('',#18008,#14288,#14289);
#12509=AXIS2_PLACEMENT_3D('',#18014,#14293,#14294);
#12510=AXIS2_PLACEMENT_3D('',#18017,#14296,#14297);
#12511=AXIS2_PLACEMENT_3D('',#18018,#14298,#14299);
#12512=AXIS2_PLACEMENT_3D('',#18022,#14301,#14302);
#12513=AXIS2_PLACEMENT_3D('',#18024,#14304,#14305);
#12514=AXIS2_PLACEMENT_3D('',#18029,#14307,#14308);
#12515=AXIS2_PLACEMENT_3D('',#18033,#14311,#14312);
#12516=AXIS2_PLACEMENT_3D('',#18034,#14313,#14314);
#12517=AXIS2_PLACEMENT_3D('',#18040,#14318,#14319);
#12518=AXIS2_PLACEMENT_3D('',#18042,#14320,#14321);
#12519=AXIS2_PLACEMENT_3D('',#18044,#14323,#14324);
#12520=AXIS2_PLACEMENT_3D('',#18045,#14325,#14326);
#12521=AXIS2_PLACEMENT_3D('',#18049,#14329,#14330);
#12522=AXIS2_PLACEMENT_3D('',#18058,#14335,#14336);
#12523=AXIS2_PLACEMENT_3D('',#18062,#14338,#14339);
#12524=AXIS2_PLACEMENT_3D('',#18069,#14340,#14341);
#12525=AXIS2_PLACEMENT_3D('',#18070,#14342,#14343);
#12526=AXIS2_PLACEMENT_3D('',#18071,#14344,#14345);
#12527=AXIS2_PLACEMENT_3D('',#18072,#14346,#14347);
#12528=AXIS2_PLACEMENT_3D('',#18073,#14348,#14349);
#12529=AXIS2_PLACEMENT_3D('',#18074,#14350,#14351);
#12530=AXIS2_PLACEMENT_3D('',#18083,#14356,#14357);
#12531=AXIS2_PLACEMENT_3D('',#18091,#14361,#14362);
#12532=AXIS2_PLACEMENT_3D('',#18092,#14363,#14364);
#12533=AXIS2_PLACEMENT_3D('',#18093,#14365,#14366);
#12534=AXIS2_PLACEMENT_3D('',#18096,#14368,#14369);
#12535=AXIS2_PLACEMENT_3D('',#18098,#14371,#14372);
#12536=AXIS2_PLACEMENT_3D('',#18105,#14375,#14376);
#12537=AXIS2_PLACEMENT_3D('',#18107,#14378,#14379);
#12538=AXIS2_PLACEMENT_3D('',#18111,#14382,#14383);
#12539=AXIS2_PLACEMENT_3D('',#18112,#14384,#14385);
#12540=AXIS2_PLACEMENT_3D('',#18113,#14386,#14387);
#12541=AXIS2_PLACEMENT_3D('',#18117,#14390,#14391);
#12542=AXIS2_PLACEMENT_3D('',#18118,#14392,#14393);
#12543=AXIS2_PLACEMENT_3D('',#18119,#14394,#14395);
#12544=AXIS2_PLACEMENT_3D('',#18120,#14396,#14397);
#12545=AXIS2_PLACEMENT_3D('',#18121,#14398,#14399);
#12546=AXIS2_PLACEMENT_3D('',#18122,#14400,#14401);
#12547=AXIS2_PLACEMENT_3D('',#18128,#14405,#14406);
#12548=AXIS2_PLACEMENT_3D('',#18132,#14409,#14410);
#12549=AXIS2_PLACEMENT_3D('',#18136,#14413,#14414);
#12550=AXIS2_PLACEMENT_3D('',#18142,#14418,#14419);
#12551=AXIS2_PLACEMENT_3D('',#18144,#14420,#14421);
#12552=AXIS2_PLACEMENT_3D('',#18147,#14423,#14424);
#12553=AXIS2_PLACEMENT_3D('',#18148,#14425,#14426);
#12554=AXIS2_PLACEMENT_3D('',#18149,#14427,#14428);
#12555=AXIS2_PLACEMENT_3D('',#18151,#14429,#14430);
#12556=AXIS2_PLACEMENT_3D('',#18153,#14432,#14433);
#12557=AXIS2_PLACEMENT_3D('',#18154,#14434,#14435);
#12558=AXIS2_PLACEMENT_3D('',#18155,#14436,#14437);
#12559=AXIS2_PLACEMENT_3D('',#18156,#14438,#14439);
#12560=AXIS2_PLACEMENT_3D('',#18159,#14442,#14443);
#12561=AXIS2_PLACEMENT_3D('',#18166,#14447,#14448);
#12562=AXIS2_PLACEMENT_3D('',#18167,#14449,#14450);
#12563=AXIS2_PLACEMENT_3D('',#18168,#14451,#14452);
#12564=AXIS2_PLACEMENT_3D('',#18172,#14455,#14456);
#12565=AXIS2_PLACEMENT_3D('',#18173,#14457,#14458);
#12566=AXIS2_PLACEMENT_3D('',#18175,#14460,#14461);
#12567=AXIS2_PLACEMENT_3D('',#18178,#14464,#14465);
#12568=AXIS2_PLACEMENT_3D('',#18179,#14466,#14467);
#12569=AXIS2_PLACEMENT_3D('',#18180,#14468,#14469);
#12570=AXIS2_PLACEMENT_3D('',#18181,#14470,#14471);
#12571=AXIS2_PLACEMENT_3D('',#18182,#14472,#14473);
#12572=AXIS2_PLACEMENT_3D('',#18185,#14474,#14475);
#12573=AXIS2_PLACEMENT_3D('',#18191,#14479,#14480);
#12574=AXIS2_PLACEMENT_3D('',#18195,#14483,#14484);
#12575=AXIS2_PLACEMENT_3D('',#18196,#14485,#14486);
#12576=AXIS2_PLACEMENT_3D('',#18197,#14487,#14488);
#12577=AXIS2_PLACEMENT_3D('',#18203,#14492,#14493);
#12578=AXIS2_PLACEMENT_3D('',#18207,#14496,#14497);
#12579=AXIS2_PLACEMENT_3D('',#18208,#14498,#14499);
#12580=AXIS2_PLACEMENT_3D('',#18210,#14501,#14502);
#12581=AXIS2_PLACEMENT_3D('',#18211,#14503,#14504);
#12582=AXIS2_PLACEMENT_3D('',#18212,#14505,#14506);
#12583=AXIS2_PLACEMENT_3D('',#18213,#14507,#14508);
#12584=AXIS2_PLACEMENT_3D('',#18214,#14509,#14510);
#12585=AXIS2_PLACEMENT_3D('',#18215,#14511,#14512);
#12586=AXIS2_PLACEMENT_3D('',#18216,#14513,#14514);
#12587=AXIS2_PLACEMENT_3D('',#18217,#14515,#14516);
#12588=AXIS2_PLACEMENT_3D('',#18218,#14517,#14518);
#12589=AXIS2_PLACEMENT_3D('',#18227,#14523,#14524);
#12590=AXIS2_PLACEMENT_3D('',#18228,#14525,#14526);
#12591=AXIS2_PLACEMENT_3D('',#18229,#14527,#14528);
#12592=AXIS2_PLACEMENT_3D('',#18238,#14533,#14534);
#12593=AXIS2_PLACEMENT_3D('',#18240,#14535,#14536);
#12594=AXIS2_PLACEMENT_3D('',#18243,#14538,#14539);
#12595=AXIS2_PLACEMENT_3D('',#18245,#14540,#14541);
#12596=AXIS2_PLACEMENT_3D('',#18248,#14543,#14544);
#12597=AXIS2_PLACEMENT_3D('',#18249,#14545,#14546);
#12598=AXIS2_PLACEMENT_3D('',#18253,#14548,#14549);
#12599=AXIS2_PLACEMENT_3D('',#18255,#14550,#14551);
#12600=AXIS2_PLACEMENT_3D('',#18258,#14553,#14554);
#12601=AXIS2_PLACEMENT_3D('',#18259,#14555,#14556);
#12602=AXIS2_PLACEMENT_3D('',#18260,#14557,#14558);
#12603=AXIS2_PLACEMENT_3D('',#18261,#14559,#14560);
#12604=AXIS2_PLACEMENT_3D('',#18262,#14561,#14562);
#12605=AXIS2_PLACEMENT_3D('',#18263,#14563,#14564);
#12606=AXIS2_PLACEMENT_3D('',#18264,#14565,#14566);
#12607=AXIS2_PLACEMENT_3D('',#18265,#14567,#14568);
#12608=AXIS2_PLACEMENT_3D('',#18266,#14569,#14570);
#12609=AXIS2_PLACEMENT_3D('',#18267,#14571,#14572);
#12610=AXIS2_PLACEMENT_3D('',#18268,#14573,#14574);
#12611=AXIS2_PLACEMENT_3D('',#18269,#14575,#14576);
#12612=AXIS2_PLACEMENT_3D('',#18270,#14577,#14578);
#12613=AXIS2_PLACEMENT_3D('',#18271,#14579,#14580);
#12614=AXIS2_PLACEMENT_3D('',#18272,#14581,#14582);
#12615=AXIS2_PLACEMENT_3D('',#18273,#14583,#14584);
#12616=AXIS2_PLACEMENT_3D('',#18274,#14585,#14586);
#12617=AXIS2_PLACEMENT_3D('',#18275,#14587,#14588);
#12618=AXIS2_PLACEMENT_3D('',#18276,#14589,#14590);
#12619=AXIS2_PLACEMENT_3D('',#18277,#14591,#14592);
#12620=AXIS2_PLACEMENT_3D('',#18278,#14593,#14594);
#12621=AXIS2_PLACEMENT_3D('',#18279,#14595,#14596);
#12622=AXIS2_PLACEMENT_3D('',#18280,#14597,#14598);
#12623=AXIS2_PLACEMENT_3D('',#18281,#14599,#14600);
#12624=AXIS2_PLACEMENT_3D('',#18282,#14601,#14602);
#12625=AXIS2_PLACEMENT_3D('',#18283,#14603,#14604);
#12626=AXIS2_PLACEMENT_3D('',#18284,#14605,#14606);
#12627=AXIS2_PLACEMENT_3D('',#18295,#14607,#14608);
#12628=AXIS2_PLACEMENT_3D('',#18318,#14609,#14610);
#12629=AXIS2_PLACEMENT_3D('',#18335,#14611,#14612);
#12630=AXIS2_PLACEMENT_3D('',#18352,#14613,#14614);
#12631=AXIS2_PLACEMENT_3D('',#18353,#14615,#14616);
#12632=AXIS2_PLACEMENT_3D('',#18354,#14617,#14618);
#12633=AXIS2_PLACEMENT_3D('',#18355,#14619,#14620);
#12634=AXIS2_PLACEMENT_3D('',#18356,#14621,#14622);
#12635=AXIS2_PLACEMENT_3D('',#18357,#14623,#14624);
#12636=AXIS2_PLACEMENT_3D('',#18430,#14625,#14626);
#12637=AXIS2_PLACEMENT_3D('',#18431,#14627,#14628);
#12638=AXIS2_PLACEMENT_3D('',#18432,#14629,#14630);
#12639=AXIS2_PLACEMENT_3D('',#18433,#14631,#14632);
#12640=AXIS2_PLACEMENT_3D('',#18434,#14633,#14634);
#12641=AXIS2_PLACEMENT_3D('',#18435,#14635,#14636);
#12642=AXIS2_PLACEMENT_3D('',#18436,#14637,#14638);
#12643=AXIS2_PLACEMENT_3D('',#18437,#14639,#14640);
#12644=AXIS2_PLACEMENT_3D('',#18444,#14641,#14642);
#12645=AXIS2_PLACEMENT_3D('',#18451,#14643,#14644);
#12646=AXIS2_PLACEMENT_3D('',#18458,#14645,#14646);
#12647=AXIS2_PLACEMENT_3D('',#18465,#14647,#14648);
#12648=AXIS2_PLACEMENT_3D('',#18466,#14649,#14650);
#12649=AXIS2_PLACEMENT_3D('',#18467,#14651,#14652);
#12650=AXIS2_PLACEMENT_3D('',#18468,#14653,#14654);
#12651=AXIS2_PLACEMENT_3D('',#18469,#14655,#14656);
#12652=AXIS2_PLACEMENT_3D('',#18470,#14657,#14658);
#12653=AXIS2_PLACEMENT_3D('',#18471,#14659,#14660);
#12654=AXIS2_PLACEMENT_3D('',#18472,#14661,#14662);
#12655=AXIS2_PLACEMENT_3D('',#18475,#14663,#14664);
#12656=AXIS2_PLACEMENT_3D('',#18479,#14666,#14667);
#12657=AXIS2_PLACEMENT_3D('',#18481,#14669,#14670);
#12658=AXIS2_PLACEMENT_3D('',#18485,#14672,#14673);
#12659=AXIS2_PLACEMENT_3D('',#18491,#14676,#14677);
#12660=AXIS2_PLACEMENT_3D('',#18497,#14680,#14681);
#12661=AXIS2_PLACEMENT_3D('',#18501,#14683,#14684);
#12662=AXIS2_PLACEMENT_3D('',#18504,#14686,#14687);
#12663=AXIS2_PLACEMENT_3D('',#18506,#14688,#14689);
#12664=AXIS2_PLACEMENT_3D('',#18508,#14690,#14691);
#12665=AXIS2_PLACEMENT_3D('',#18509,#14692,#14693);
#12666=AXIS2_PLACEMENT_3D('',#18513,#14696,#14697);
#12667=AXIS2_PLACEMENT_3D('',#18516,#14698,#14699);
#12668=AXIS2_PLACEMENT_3D('',#18520,#14701,#14702);
#12669=AXIS2_PLACEMENT_3D('',#18522,#14704,#14705);
#12670=AXIS2_PLACEMENT_3D('',#18526,#14707,#14708);
#12671=AXIS2_PLACEMENT_3D('',#18532,#14711,#14712);
#12672=AXIS2_PLACEMENT_3D('',#18538,#14715,#14716);
#12673=AXIS2_PLACEMENT_3D('',#18546,#14720,#14721);
#12674=AXIS2_PLACEMENT_3D('',#18549,#14723,#14724);
#12675=AXIS2_PLACEMENT_3D('',#18551,#14725,#14726);
#12676=AXIS2_PLACEMENT_3D('',#18553,#14727,#14728);
#12677=AXIS2_PLACEMENT_3D('',#18555,#14729,#14730);
#12678=AXIS2_PLACEMENT_3D('',#18556,#14731,#14732);
#12679=AXIS2_PLACEMENT_3D('',#18560,#14735,#14736);
#12680=AXIS2_PLACEMENT_3D('',#18562,#14737,#14738);
#12681=AXIS2_PLACEMENT_3D('',#18564,#14740,#14741);
#12682=AXIS2_PLACEMENT_3D('',#18568,#14744,#14745);
#12683=AXIS2_PLACEMENT_3D('',#18570,#14746,#14747);
#12684=AXIS2_PLACEMENT_3D('',#18572,#14749,#14750);
#12685=AXIS2_PLACEMENT_3D('',#18576,#14753,#14754);
#12686=AXIS2_PLACEMENT_3D('',#18589,#14757,#14758);
#12687=AXIS2_PLACEMENT_3D('',#18591,#14759,#14760);
#12688=AXIS2_PLACEMENT_3D('',#18595,#14762,#14763);
#12689=AXIS2_PLACEMENT_3D('',#18599,#14765,#14766);
#12690=AXIS2_PLACEMENT_3D('',#18604,#14769,#14770);
#12691=AXIS2_PLACEMENT_3D('',#18606,#14771,#14772);
#12692=AXIS2_PLACEMENT_3D('',#18608,#14773,#14774);
#12693=AXIS2_PLACEMENT_3D('',#18609,#14775,#14776);
#12694=AXIS2_PLACEMENT_3D('',#18618,#14779,#14780);
#12695=AXIS2_PLACEMENT_3D('',#18620,#14781,#14782);
#12696=AXIS2_PLACEMENT_3D('',#18623,#14784,#14785);
#12697=AXIS2_PLACEMENT_3D('',#18624,#14786,#14787);
#12698=AXIS2_PLACEMENT_3D('',#18627,#14788,#14789);
#12699=AXIS2_PLACEMENT_3D('',#18628,#14790,#14791);
#12700=AXIS2_PLACEMENT_3D('',#18631,#14793,#14794);
#12701=AXIS2_PLACEMENT_3D('',#18632,#14795,#14796);
#12702=AXIS2_PLACEMENT_3D('',#18634,#14797,#14798);
#12703=AXIS2_PLACEMENT_3D('',#18640,#14799,#14800);
#12704=AXIS2_PLACEMENT_3D('',#18641,#14801,#14802);
#12705=AXIS2_PLACEMENT_3D('',#18643,#14803,#14804);
#12706=AXIS2_PLACEMENT_3D('',#18645,#14805,#14806);
#12707=AXIS2_PLACEMENT_3D('',#18654,#14807,#14808);
#12708=AXIS2_PLACEMENT_3D('',#18656,#14810,#14811);
#12709=AXIS2_PLACEMENT_3D('',#18658,#14813,#14814);
#12710=AXIS2_PLACEMENT_3D('',#18660,#14815,#14816);
#12711=AXIS2_PLACEMENT_3D('',#18662,#14818,#14819);
#12712=AXIS2_PLACEMENT_3D('',#18665,#14821,#14822);
#12713=AXIS2_PLACEMENT_3D('',#18667,#14824,#14825);
#12714=AXIS2_PLACEMENT_3D('',#18669,#14826,#14827);
#12715=AXIS2_PLACEMENT_3D('',#18671,#14829,#14830);
#12716=AXIS2_PLACEMENT_3D('',#18673,#14831,#14832);
#12717=AXIS2_PLACEMENT_3D('',#18675,#14834,#14835);
#12718=AXIS2_PLACEMENT_3D('',#18677,#14836,#14837);
#12719=AXIS2_PLACEMENT_3D('',#18680,#14839,#14840);
#12720=AXIS2_PLACEMENT_3D('',#18681,#14841,#14842);
#12721=AXIS2_PLACEMENT_3D('',#18684,#14845,#14846);
#12722=AXIS2_PLACEMENT_3D('',#18693,#14851,#14852);
#12723=AXIS2_PLACEMENT_3D('',#18719,#14856,#14857);
#12724=AXIS2_PLACEMENT_3D('',#18721,#14859,#14860);
#12725=AXIS2_PLACEMENT_3D('',#18738,#14863,#14864);
#12726=AXIS2_PLACEMENT_3D('',#18751,#14867,#14868);
#12727=AXIS2_PLACEMENT_3D('',#18753,#14870,#14871);
#12728=AXIS2_PLACEMENT_3D('',#18757,#14874,#14875);
#12729=AXIS2_PLACEMENT_3D('',#18761,#14878,#14879);
#12730=AXIS2_PLACEMENT_3D('',#18763,#14881,#14882);
#12731=AXIS2_PLACEMENT_3D('',#18766,#14885,#14886);
#12732=AXIS2_PLACEMENT_3D('',#18768,#14888,#14889);
#12733=AXIS2_PLACEMENT_3D('',#18769,#14890,#14891);
#12734=AXIS2_PLACEMENT_3D('',#18770,#14892,#14893);
#12735=AXIS2_PLACEMENT_3D('',#18776,#14897,#14898);
#12736=AXIS2_PLACEMENT_3D('',#18777,#14899,#14900);
#12737=AXIS2_PLACEMENT_3D('',#18778,#14901,#14902);
#12738=AXIS2_PLACEMENT_3D('',#18779,#14903,#14904);
#12739=AXIS2_PLACEMENT_3D('',#18780,#14905,#14906);
#12740=AXIS2_PLACEMENT_3D('',#18781,#14907,#14908);
#12741=AXIS2_PLACEMENT_3D('',#18782,#14909,#14910);
#12742=AXIS2_PLACEMENT_3D('',#18783,#14911,#14912);
#12743=AXIS2_PLACEMENT_3D('',#18784,#14913,#14914);
#12744=AXIS2_PLACEMENT_3D('',#18785,#14915,#14916);
#12745=AXIS2_PLACEMENT_3D('',#18786,#14917,#14918);
#12746=AXIS2_PLACEMENT_3D('',#18787,#14919,#14920);
#12747=AXIS2_PLACEMENT_3D('',#18788,#14921,#14922);
#12748=AXIS2_PLACEMENT_3D('',#18789,#14923,#14924);
#12749=AXIS2_PLACEMENT_3D('',#18790,#14925,#14926);
#12750=AXIS2_PLACEMENT_3D('',#18791,#14927,#14928);
#12751=AXIS2_PLACEMENT_3D('',#18793,#14929,#14930);
#12752=AXIS2_PLACEMENT_3D('',#18796,#14932,#14933);
#12753=AXIS2_PLACEMENT_3D('',#18797,#14934,#14935);
#12754=AXIS2_PLACEMENT_3D('',#18799,#14936,#14937);
#12755=AXIS2_PLACEMENT_3D('',#18802,#14939,#14940);
#12756=AXIS2_PLACEMENT_3D('',#18803,#14941,#14942);
#12757=AXIS2_PLACEMENT_3D('',#18806,#14943,#14944);
#12758=AXIS2_PLACEMENT_3D('',#18807,#14945,#14946);
#12759=AXIS2_PLACEMENT_3D('',#18810,#14948,#14949);
#12760=AXIS2_PLACEMENT_3D('',#18811,#14950,#14951);
#12761=AXIS2_PLACEMENT_3D('',#18813,#14952,#14953);
#12762=AXIS2_PLACEMENT_3D('',#18815,#14955,#14956);
#12763=AXIS2_PLACEMENT_3D('',#18817,#14958,#14959);
#12764=AXIS2_PLACEMENT_3D('',#18818,#14960,#14961);
#12765=AXIS2_PLACEMENT_3D('',#18819,#14962,#14963);
#12766=AXIS2_PLACEMENT_3D('',#18820,#14964,#14965);
#12767=AXIS2_PLACEMENT_3D('',#18822,#14966,#14967);
#12768=AXIS2_PLACEMENT_3D('',#18825,#14969,#14970);
#12769=AXIS2_PLACEMENT_3D('',#18826,#14971,#14972);
#12770=AXIS2_PLACEMENT_3D('',#18828,#14973,#14974);
#12771=AXIS2_PLACEMENT_3D('',#18831,#14976,#14977);
#12772=AXIS2_PLACEMENT_3D('',#18832,#14978,#14979);
#12773=AXIS2_PLACEMENT_3D('',#18835,#14980,#14981);
#12774=AXIS2_PLACEMENT_3D('',#18838,#14983,#14984);
#12775=AXIS2_PLACEMENT_3D('',#18839,#14985,#14986);
#12776=AXIS2_PLACEMENT_3D('',#18840,#14987,#14988);
#12777=AXIS2_PLACEMENT_3D('',#18842,#14989,#14990);
#12778=AXIS2_PLACEMENT_3D('',#18844,#14992,#14993);
#12779=AXIS2_PLACEMENT_3D('',#18846,#14995,#14996);
#12780=AXIS2_PLACEMENT_3D('',#18847,#14997,#14998);
#12781=AXIS2_PLACEMENT_3D('',#18848,#14999,#15000);
#12782=AXIS2_PLACEMENT_3D('',#18849,#15001,#15002);
#12783=AXIS2_PLACEMENT_3D('',#18850,#15003,#15004);
#12784=AXIS2_PLACEMENT_3D('',#18851,#15005,#15006);
#12785=AXIS2_PLACEMENT_3D('',#18852,#15007,#15008);
#12786=AXIS2_PLACEMENT_3D('',#18853,#15009,#15010);
#12787=AXIS2_PLACEMENT_3D('',#18856,#15011,#15012);
#12788=AXIS2_PLACEMENT_3D('',#18857,#15013,#15014);
#12789=AXIS2_PLACEMENT_3D('',#18860,#15016,#15017);
#12790=AXIS2_PLACEMENT_3D('',#18861,#15018,#15019);
#12791=AXIS2_PLACEMENT_3D('',#18864,#15020,#15021);
#12792=AXIS2_PLACEMENT_3D('',#18870,#15022,#15023);
#12793=AXIS2_PLACEMENT_3D('',#18874,#15024,#15025);
#12794=AXIS2_PLACEMENT_3D('',#18877,#15026,#15027);
#12795=AXIS2_PLACEMENT_3D('',#18879,#15028,#15029);
#12796=AXIS2_PLACEMENT_3D('',#18881,#15030,#15031);
#12797=AXIS2_PLACEMENT_3D('',#18883,#15032,#15033);
#12798=AXIS2_PLACEMENT_3D('',#18885,#15034,#15035);
#12799=AXIS2_PLACEMENT_3D('',#18887,#15036,#15037);
#12800=AXIS2_PLACEMENT_3D('',#18889,#15038,#15039);
#12801=AXIS2_PLACEMENT_3D('',#18891,#15040,#15041);
#12802=AXIS2_PLACEMENT_3D('',#18893,#15042,#15043);
#12803=AXIS2_PLACEMENT_3D('',#18895,#15044,#15045);
#12804=AXIS2_PLACEMENT_3D('',#18897,#15046,#15047);
#12805=AXIS2_PLACEMENT_3D('',#18899,#15048,#15049);
#12806=AXIS2_PLACEMENT_3D('',#18901,#15050,#15051);
#12807=AXIS2_PLACEMENT_3D('',#18903,#15052,#15053);
#12808=AXIS2_PLACEMENT_3D('',#18905,#15054,#15055);
#12809=AXIS2_PLACEMENT_3D('',#18906,#15056,#15057);
#12810=AXIS2_PLACEMENT_3D('',#18907,#15058,#15059);
#12811=AXIS2_PLACEMENT_3D('',#18910,#15060,#15061);
#12812=AXIS2_PLACEMENT_3D('',#18912,#15062,#15063);
#12813=AXIS2_PLACEMENT_3D('',#18914,#15064,#15065);
#12814=AXIS2_PLACEMENT_3D('',#18915,#15066,#15067);
#12815=AXIS2_PLACEMENT_3D('',#18917,#15068,#15069);
#12816=AXIS2_PLACEMENT_3D('',#18919,#15070,#15071);
#12817=AXIS2_PLACEMENT_3D('',#18921,#15072,#15073);
#12818=AXIS2_PLACEMENT_3D('',#18923,#15074,#15075);
#12819=AXIS2_PLACEMENT_3D('',#18925,#15076,#15077);
#12820=AXIS2_PLACEMENT_3D('',#18927,#15078,#15079);
#12821=AXIS2_PLACEMENT_3D('',#18929,#15080,#15081);
#12822=AXIS2_PLACEMENT_3D('',#18931,#15082,#15083);
#12823=AXIS2_PLACEMENT_3D('',#18933,#15084,#15085);
#12824=AXIS2_PLACEMENT_3D('',#18935,#15086,#15087);
#12825=AXIS2_PLACEMENT_3D('',#18936,#15088,#15089);
#12826=AXIS2_PLACEMENT_3D('',#18938,#15090,#15091);
#12827=AXIS2_PLACEMENT_3D('',#18939,#15092,#15093);
#12828=AXIS2_PLACEMENT_3D('',#18941,#15095,#15096);
#12829=AXIS2_PLACEMENT_3D('',#18947,#15097,#15098);
#12830=AXIS2_PLACEMENT_3D('',#18951,#15099,#15100);
#12831=AXIS2_PLACEMENT_3D('',#18957,#15101,#15102);
#12832=AXIS2_PLACEMENT_3D('',#18961,#15103,#15104);
#12833=AXIS2_PLACEMENT_3D('',#18967,#15105,#15106);
#12834=AXIS2_PLACEMENT_3D('',#18971,#15107,#15108);
#12835=AXIS2_PLACEMENT_3D('',#18972,#15109,#15110);
#12836=AXIS2_PLACEMENT_3D('',#18978,#15111,#15112);
#12837=AXIS2_PLACEMENT_3D('',#18982,#15113,#15114);
#12838=AXIS2_PLACEMENT_3D('',#18986,#15116,#15117);
#12839=AXIS2_PLACEMENT_3D('',#18988,#15119,#15120);
#12840=AXIS2_PLACEMENT_3D('',#18993,#15122,#15123);
#12841=AXIS2_PLACEMENT_3D('',#18998,#15125,#15126);
#12842=AXIS2_PLACEMENT_3D('',#19005,#15129,#15130);
#12843=AXIS2_PLACEMENT_3D('',#19012,#15133,#15134);
#12844=AXIS2_PLACEMENT_3D('',#19013,#15135,#15136);
#12845=AXIS2_PLACEMENT_3D('',#19014,#15137,#15138);
#12846=AXIS2_PLACEMENT_3D('',#19017,#15141,#15142);
#12847=AXIS2_PLACEMENT_3D('',#19019,#15144,#15145);
#12848=AXIS2_PLACEMENT_3D('',#19021,#15147,#15148);
#12849=AXIS2_PLACEMENT_3D('',#19028,#15151,#15152);
#12850=AXIS2_PLACEMENT_3D('',#19035,#15155,#15156);
#12851=AXIS2_PLACEMENT_3D('',#19036,#15157,#15158);
#12852=AXIS2_PLACEMENT_3D('',#19037,#15159,#15160);
#12853=AXIS2_PLACEMENT_3D('',#19038,#15161,#15162);
#12854=AXIS2_PLACEMENT_3D('',#19039,#15163,#15164);
#12855=AXIS2_PLACEMENT_3D('',#19040,#15165,#15166);
#12856=AXIS2_PLACEMENT_3D('',#19041,#15167,#15168);
#12857=AXIS2_PLACEMENT_3D('',#19042,#15169,#15170);
#12858=AXIS2_PLACEMENT_3D('',#19043,#15171,#15172);
#12859=AXIS2_PLACEMENT_3D('',#19044,#15173,#15174);
#12860=AXIS2_PLACEMENT_3D('',#19045,#15175,#15176);
#12861=AXIS2_PLACEMENT_3D('',#19047,#15177,#15178);
#12862=AXIS2_PLACEMENT_3D('',#19050,#15180,#15181);
#12863=AXIS2_PLACEMENT_3D('',#19051,#15182,#15183);
#12864=AXIS2_PLACEMENT_3D('',#19053,#15184,#15185);
#12865=AXIS2_PLACEMENT_3D('',#19055,#15186,#15187);
#12866=AXIS2_PLACEMENT_3D('',#19057,#15188,#15189);
#12867=AXIS2_PLACEMENT_3D('',#19058,#15190,#15191);
#12868=AXIS2_PLACEMENT_3D('',#19059,#15192,#15193);
#12869=AXIS2_PLACEMENT_3D('',#19061,#15194,#15195);
#12870=AXIS2_PLACEMENT_3D('',#19063,#15196,#15197);
#12871=AXIS2_PLACEMENT_3D('',#19065,#15198,#15199);
#12872=AXIS2_PLACEMENT_3D('',#19066,#15200,#15201);
#12873=AXIS2_PLACEMENT_3D('',#19067,#15202,#15203);
#12874=AXIS2_PLACEMENT_3D('',#19069,#15205,#15206);
#12875=AXIS2_PLACEMENT_3D('',#19071,#15207,#15208);
#12876=AXIS2_PLACEMENT_3D('',#19074,#15210,#15211);
#12877=AXIS2_PLACEMENT_3D('',#19075,#15212,#15213);
#12878=AXIS2_PLACEMENT_3D('',#19093,#15214,#15215);
#12879=AXIS2_PLACEMENT_3D('',#19105,#15217,#15218);
#12880=AXIS2_PLACEMENT_3D('',#19115,#15219,#15220);
#12881=AXIS2_PLACEMENT_3D('',#19116,#15221,#15222);
#12882=AXIS2_PLACEMENT_3D('',#19118,#15223,#15224);
#12883=AXIS2_PLACEMENT_3D('',#19121,#15226,#15227);
#12884=AXIS2_PLACEMENT_3D('',#19122,#15228,#15229);
#12885=AXIS2_PLACEMENT_3D('',#19124,#15230,#15231);
#12886=AXIS2_PLACEMENT_3D('',#19126,#15233,#15234);
#12887=AXIS2_PLACEMENT_3D('',#19128,#15235,#15236);
#12888=AXIS2_PLACEMENT_3D('',#19131,#15238,#15239);
#12889=AXIS2_PLACEMENT_3D('',#19132,#15240,#15241);
#12890=AXIS2_PLACEMENT_3D('',#19134,#15242,#15243);
#12891=AXIS2_PLACEMENT_3D('',#19137,#15245,#15246);
#12892=AXIS2_PLACEMENT_3D('',#19138,#15247,#15248);
#12893=AXIS2_PLACEMENT_3D('',#19141,#15249,#15250);
#12894=AXIS2_PLACEMENT_3D('',#19145,#15252,#15253);
#12895=AXIS2_PLACEMENT_3D('',#19147,#15255,#15256);
#12896=AXIS2_PLACEMENT_3D('',#19149,#15257,#15258);
#12897=AXIS2_PLACEMENT_3D('',#19152,#15260,#15261);
#12898=AXIS2_PLACEMENT_3D('',#19153,#15262,#15263);
#12899=AXIS2_PLACEMENT_3D('',#19156,#15264,#15265);
#12900=AXIS2_PLACEMENT_3D('',#19160,#15267,#15268);
#12901=AXIS2_PLACEMENT_3D('',#19162,#15270,#15271);
#12902=AXIS2_PLACEMENT_3D('',#19166,#15273,#15274);
#12903=AXIS2_PLACEMENT_3D('',#19170,#15276,#15277);
#12904=AXIS2_PLACEMENT_3D('',#19172,#15279,#15280);
#12905=AXIS2_PLACEMENT_3D('',#19176,#15283,#15284);
#12906=AXIS2_PLACEMENT_3D('',#19178,#15285,#15286);
#12907=AXIS2_PLACEMENT_3D('',#19182,#15288,#15289);
#12908=AXIS2_PLACEMENT_3D('',#19184,#15291,#15292);
#12909=AXIS2_PLACEMENT_3D('',#19190,#15296,#15297);
#12910=AXIS2_PLACEMENT_3D('',#19196,#15301,#15302);
#12911=AXIS2_PLACEMENT_3D('',#19200,#15304,#15305);
#12912=AXIS2_PLACEMENT_3D('',#19208,#15309,#15310);
#12913=AXIS2_PLACEMENT_3D('',#19210,#15312,#15313);
#12914=AXIS2_PLACEMENT_3D('',#19214,#15315,#15316);
#12915=AXIS2_PLACEMENT_3D('',#19216,#15317,#15318);
#12916=AXIS2_PLACEMENT_3D('',#19220,#15321,#15322);
#12917=AXIS2_PLACEMENT_3D('',#19229,#15327,#15328);
#12918=AXIS2_PLACEMENT_3D('',#19234,#15331,#15332);
#12919=AXIS2_PLACEMENT_3D('',#19235,#15333,#15334);
#12920=AXIS2_PLACEMENT_3D('',#19246,#15341,#15342);
#12921=AXIS2_PLACEMENT_3D('',#19250,#15345,#15346);
#12922=AXIS2_PLACEMENT_3D('',#19254,#15349,#15350);
#12923=AXIS2_PLACEMENT_3D('',#19259,#15353,#15354);
#12924=AXIS2_PLACEMENT_3D('',#19260,#15355,#15356);
#12925=AXIS2_PLACEMENT_3D('',#19272,#15364,#15365);
#12926=AXIS2_PLACEMENT_3D('',#19273,#15366,#15367);
#12927=AXIS2_PLACEMENT_3D('',#19274,#15368,#15369);
#12928=AXIS2_PLACEMENT_3D('',#19277,#15372,#15373);
#12929=AXIS2_PLACEMENT_3D('',#19278,#15374,#15375);
#12930=AXIS2_PLACEMENT_3D('',#19279,#15376,#15377);
#12931=AXIS2_PLACEMENT_3D('',#19280,#15378,#15379);
#12932=AXIS2_PLACEMENT_3D('',#19281,#15380,#15381);
#12933=AXIS2_PLACEMENT_3D('',#19282,#15382,#15383);
#12934=AXIS2_PLACEMENT_3D('',#19283,#15384,#15385);
#12935=AXIS2_PLACEMENT_3D('',#19286,#15388,#15389);
#12936=AXIS2_PLACEMENT_3D('',#19287,#15390,#15391);
#12937=AXIS2_PLACEMENT_3D('',#19288,#15392,#15393);
#12938=AXIS2_PLACEMENT_3D('',#19289,#15394,#15395);
#12939=AXIS2_PLACEMENT_3D('',#19290,#15396,#15397);
#12940=AXIS2_PLACEMENT_3D('',#19291,#15398,#15399);
#12941=AXIS2_PLACEMENT_3D('',#19292,#15400,#15401);
#12942=AXIS2_PLACEMENT_3D('',#19293,#15402,#15403);
#12943=AXIS2_PLACEMENT_3D('',#19294,#15404,#15405);
#12944=AXIS2_PLACEMENT_3D('',#19295,#15406,#15407);
#12945=AXIS2_PLACEMENT_3D('',#19296,#15408,#15409);
#12946=AXIS2_PLACEMENT_3D('',#19298,#15410,#15411);
#12947=AXIS2_PLACEMENT_3D('',#19301,#15413,#15414);
#12948=AXIS2_PLACEMENT_3D('',#19302,#15415,#15416);
#12949=AXIS2_PLACEMENT_3D('',#19305,#15417,#15418);
#12950=AXIS2_PLACEMENT_3D('',#19306,#15419,#15420);
#12951=AXIS2_PLACEMENT_3D('',#19309,#15422,#15423);
#12952=AXIS2_PLACEMENT_3D('',#19310,#15424,#15425);
#12953=AXIS2_PLACEMENT_3D('',#19312,#15427,#15428);
#12954=AXIS2_PLACEMENT_3D('',#19313,#15429,#15430);
#12955=AXIS2_PLACEMENT_3D('',#19314,#15431,#15432);
#12956=AXIS2_PLACEMENT_3D('',#19316,#15433,#15434);
#12957=AXIS2_PLACEMENT_3D('',#19319,#15436,#15437);
#12958=AXIS2_PLACEMENT_3D('',#19320,#15438,#15439);
#12959=AXIS2_PLACEMENT_3D('',#19323,#15440,#15441);
#12960=AXIS2_PLACEMENT_3D('',#19324,#15442,#15443);
#12961=AXIS2_PLACEMENT_3D('',#19327,#15445,#15446);
#12962=AXIS2_PLACEMENT_3D('',#19328,#15447,#15448);
#12963=AXIS2_PLACEMENT_3D('',#19330,#15450,#15451);
#12964=AXIS2_PLACEMENT_3D('',#19331,#15452,#15453);
#12965=AXIS2_PLACEMENT_3D('',#19332,#15454,#15455);
#12966=AXIS2_PLACEMENT_3D('',#19333,#15456,#15457);
#12967=AXIS2_PLACEMENT_3D('',#19334,#15458,#15459);
#12968=AXIS2_PLACEMENT_3D('',#19335,#15460,#15461);
#12969=AXIS2_PLACEMENT_3D('',#19336,#15462,#15463);
#12970=AXIS2_PLACEMENT_3D('',#19338,#15464,#15465);
#12971=AXIS2_PLACEMENT_3D('',#19341,#15467,#15468);
#12972=AXIS2_PLACEMENT_3D('',#19342,#15469,#15470);
#12973=AXIS2_PLACEMENT_3D('',#19344,#15471,#15472);
#12974=AXIS2_PLACEMENT_3D('',#19347,#15474,#15475);
#12975=AXIS2_PLACEMENT_3D('',#19348,#15476,#15477);
#12976=AXIS2_PLACEMENT_3D('',#19353,#15479,#15480);
#12977=AXIS2_PLACEMENT_3D('',#19357,#15482,#15483);
#12978=AXIS2_PLACEMENT_3D('',#19361,#15485,#15486);
#12979=AXIS2_PLACEMENT_3D('',#19364,#15488,#15489);
#12980=AXIS2_PLACEMENT_3D('',#19365,#15490,#15491);
#12981=AXIS2_PLACEMENT_3D('',#19370,#15493,#15494);
#12982=AXIS2_PLACEMENT_3D('',#19374,#15496,#15497);
#12983=AXIS2_PLACEMENT_3D('',#19378,#15499,#15500);
#12984=AXIS2_PLACEMENT_3D('',#19381,#15502,#15503);
#12985=AXIS2_PLACEMENT_3D('',#19382,#15504,#15505);
#12986=AXIS2_PLACEMENT_3D('',#19385,#15508,#15509);
#12987=AXIS2_PLACEMENT_3D('',#19388,#15512,#15513);
#12988=AXIS2_PLACEMENT_3D('',#19391,#15516,#15517);
#12989=AXIS2_PLACEMENT_3D('',#19394,#15520,#15521);
#12990=AXIS2_PLACEMENT_3D('',#19395,#15522,#15523);
#12991=AXIS2_PLACEMENT_3D('',#19396,#15524,#15525);
#12992=AXIS2_PLACEMENT_3D('',#19397,#15526,#15527);
#12993=AXIS2_PLACEMENT_3D('',#19398,#15528,#15529);
#12994=AXIS2_PLACEMENT_3D('',#19399,#15530,#15531);
#12995=AXIS2_PLACEMENT_3D('',#19400,#15532,#15533);
#12996=AXIS2_PLACEMENT_3D('',#19423,#15535,#15536);
#12997=AXIS2_PLACEMENT_3D('',#19442,#15537,#15538);
#12998=AXIS2_PLACEMENT_3D('',#19444,#15539,#15540);
#12999=AXIS2_PLACEMENT_3D('',#19446,#15541,#15542);
#13000=AXIS2_PLACEMENT_3D('',#19448,#15543,#15544);
#13001=AXIS2_PLACEMENT_3D('',#19449,#15545,#15546);
#13002=AXIS2_PLACEMENT_3D('',#19450,#15547,#15548);
#13003=AXIS2_PLACEMENT_3D('',#19453,#15549,#15550);
#13004=AXIS2_PLACEMENT_3D('',#19454,#15551,#15552);
#13005=AXIS2_PLACEMENT_3D('',#19456,#15553,#15554);
#13006=AXIS2_PLACEMENT_3D('',#19457,#15555,#15556);
#13007=AXIS2_PLACEMENT_3D('',#19458,#15557,#15558);
#13008=AXIS2_PLACEMENT_3D('',#19460,#15559,#15560);
#13009=AXIS2_PLACEMENT_3D('',#19463,#15562,#15563);
#13010=AXIS2_PLACEMENT_3D('',#19464,#15564,#15565);
#13011=AXIS2_PLACEMENT_3D('',#19466,#15566,#15567);
#13012=AXIS2_PLACEMENT_3D('',#19469,#15569,#15570);
#13013=AXIS2_PLACEMENT_3D('',#19470,#15571,#15572);
#13014=AXIS2_PLACEMENT_3D('',#19472,#15573,#15574);
#13015=AXIS2_PLACEMENT_3D('',#19475,#15576,#15577);
#13016=AXIS2_PLACEMENT_3D('',#19476,#15578,#15579);
#13017=AXIS2_PLACEMENT_3D('',#19478,#15580,#15581);
#13018=AXIS2_PLACEMENT_3D('',#19481,#15583,#15584);
#13019=AXIS2_PLACEMENT_3D('',#19482,#15585,#15586);
#13020=AXIS2_PLACEMENT_3D('',#19485,#15587,#15588);
#13021=AXIS2_PLACEMENT_3D('',#19487,#15589,#15590);
#13022=AXIS2_PLACEMENT_3D('',#19491,#15592,#15593);
#13023=AXIS2_PLACEMENT_3D('',#19493,#15594,#15595);
#13024=AXIS2_PLACEMENT_3D('',#19496,#15597,#15598);
#13025=AXIS2_PLACEMENT_3D('',#19497,#15599,#15600);
#13026=AXIS2_PLACEMENT_3D('',#19500,#15601,#15602);
#13027=AXIS2_PLACEMENT_3D('',#19502,#15603,#15604);
#13028=AXIS2_PLACEMENT_3D('',#19506,#15606,#15607);
#13029=AXIS2_PLACEMENT_3D('',#19508,#15608,#15609);
#13030=AXIS2_PLACEMENT_3D('',#19510,#15610,#15611);
#13031=AXIS2_PLACEMENT_3D('',#19512,#15613,#15614);
#13032=AXIS2_PLACEMENT_3D('',#19514,#15615,#15616);
#13033=AXIS2_PLACEMENT_3D('',#19518,#15618,#15619);
#13034=AXIS2_PLACEMENT_3D('',#19520,#15620,#15621);
#13035=AXIS2_PLACEMENT_3D('',#19522,#15622,#15623);
#13036=AXIS2_PLACEMENT_3D('',#19524,#15624,#15625);
#13037=AXIS2_PLACEMENT_3D('',#19526,#15626,#15627);
#13038=AXIS2_PLACEMENT_3D('',#19527,#15628,#15629);
#13039=AXIS2_PLACEMENT_3D('',#19528,#15630,#15631);
#13040=AXIS2_PLACEMENT_3D('',#19531,#15632,#15633);
#13041=AXIS2_PLACEMENT_3D('',#19535,#15635,#15636);
#13042=AXIS2_PLACEMENT_3D('',#19537,#15638,#15639);
#13043=AXIS2_PLACEMENT_3D('',#19539,#15640,#15641);
#13044=AXIS2_PLACEMENT_3D('',#19542,#15643,#15644);
#13045=AXIS2_PLACEMENT_3D('',#19543,#15645,#15646);
#13046=AXIS2_PLACEMENT_3D('',#19545,#15647,#15648);
#13047=AXIS2_PLACEMENT_3D('',#19548,#15650,#15651);
#13048=AXIS2_PLACEMENT_3D('',#19549,#15652,#15653);
#13049=AXIS2_PLACEMENT_3D('',#19551,#15654,#15655);
#13050=AXIS2_PLACEMENT_3D('',#19554,#15657,#15658);
#13051=AXIS2_PLACEMENT_3D('',#19555,#15659,#15660);
#13052=AXIS2_PLACEMENT_3D('',#19557,#15661,#15662);
#13053=AXIS2_PLACEMENT_3D('',#19561,#15664,#15665);
#13054=AXIS2_PLACEMENT_3D('',#19563,#15666,#15667);
#13055=AXIS2_PLACEMENT_3D('',#19564,#15668,#15669);
#13056=AXIS2_PLACEMENT_3D('',#19565,#15670,#15671);
#13057=AXIS2_PLACEMENT_3D('',#19568,#15672,#15673);
#13058=AXIS2_PLACEMENT_3D('',#19575,#15675,#15676);
#13059=AXIS2_PLACEMENT_3D('',#19577,#15677,#15678);
#13060=AXIS2_PLACEMENT_3D('',#19579,#15679,#15680);
#13061=AXIS2_PLACEMENT_3D('',#19581,#15681,#15682);
#13062=AXIS2_PLACEMENT_3D('',#19582,#15683,#15684);
#13063=AXIS2_PLACEMENT_3D('',#19587,#15685,#15686);
#13064=AXIS2_PLACEMENT_3D('',#19932,#15691,#15692);
#13065=AXIS2_PLACEMENT_3D('',#19941,#15697,#15698);
#13066=AXIS2_PLACEMENT_3D('',#20037,#15700,#15701);
#13067=AXIS2_PLACEMENT_3D('',#20043,#15705,#15706);
#13068=AXIS2_PLACEMENT_3D('',#20044,#15707,#15708);
#13069=AXIS2_PLACEMENT_3D('',#20045,#15709,#15710);
#13070=AXIS2_PLACEMENT_3D('',#20046,#15711,#15712);
#13071=AXIS2_PLACEMENT_3D('',#20047,#15713,#15714);
#13072=AXIS2_PLACEMENT_3D('',#20048,#15715,#15716);
#13073=AXIS2_PLACEMENT_3D('',#20049,#15717,#15718);
#13074=AXIS2_PLACEMENT_3D('',#20050,#15719,#15720);
#13075=AXIS2_PLACEMENT_3D('',#20051,#15721,#15722);
#13076=AXIS2_PLACEMENT_3D('',#20052,#15723,#15724);
#13077=AXIS2_PLACEMENT_3D('',#20053,#15725,#15726);
#13078=AXIS2_PLACEMENT_3D('',#20054,#15727,#15728);
#13079=AXIS2_PLACEMENT_3D('',#20067,#15735,#15736);
#13080=AXIS2_PLACEMENT_3D('',#20073,#15740,#15741);
#13081=AXIS2_PLACEMENT_3D('',#20077,#15744,#15745);
#13082=AXIS2_PLACEMENT_3D('',#20081,#15748,#15749);
#13083=AXIS2_PLACEMENT_3D('',#20085,#15752,#15753);
#13084=AXIS2_PLACEMENT_3D('',#20089,#15756,#15757);
#13085=AXIS2_PLACEMENT_3D('',#20091,#15759,#15760);
#13086=AXIS2_PLACEMENT_3D('',#20104,#15767,#15768);
#13087=AXIS2_PLACEMENT_3D('',#20118,#15776,#15777);
#13088=AXIS2_PLACEMENT_3D('',#20126,#15783,#15784);
#13089=AXIS2_PLACEMENT_3D('',#20128,#15786,#15787);
#13090=AXIS2_PLACEMENT_3D('',#20130,#15789,#15790);
#13091=AXIS2_PLACEMENT_3D('',#20131,#15791,#15792);
#13092=AXIS2_PLACEMENT_3D('',#20135,#15794,#15795);
#13093=AXIS2_PLACEMENT_3D('',#20137,#15797,#15798);
#13094=AXIS2_PLACEMENT_3D('',#20141,#15801,#15802);
#13095=AXIS2_PLACEMENT_3D('',#20144,#15804,#15805);
#13096=AXIS2_PLACEMENT_3D('',#20145,#15806,#15807);
#13097=AXIS2_PLACEMENT_3D('',#20147,#15809,#15810);
#13098=AXIS2_PLACEMENT_3D('',#20151,#15813,#15814);
#13099=AXIS2_PLACEMENT_3D('',#20155,#15817,#15818);
#13100=AXIS2_PLACEMENT_3D('',#20159,#15821,#15822);
#13101=AXIS2_PLACEMENT_3D('',#20163,#15825,#15826);
#13102=AXIS2_PLACEMENT_3D('',#20167,#15829,#15830);
#13103=AXIS2_PLACEMENT_3D('',#20171,#15833,#15834);
#13104=AXIS2_PLACEMENT_3D('',#20175,#15836,#15837);
#13105=AXIS2_PLACEMENT_3D('',#20178,#15840,#15841);
#13106=AXIS2_PLACEMENT_3D('',#20183,#15844,#15845);
#13107=AXIS2_PLACEMENT_3D('',#20184,#15846,#15847);
#13108=AXIS2_PLACEMENT_3D('',#20188,#15849,#15850);
#13109=AXIS2_PLACEMENT_3D('',#20191,#15852,#15853);
#13110=AXIS2_PLACEMENT_3D('',#20192,#15854,#15855);
#13111=AXIS2_PLACEMENT_3D('',#20195,#15857,#15858);
#13112=AXIS2_PLACEMENT_3D('',#20197,#15860,#15861);
#13113=AXIS2_PLACEMENT_3D('',#20201,#15863,#15864);
#13114=AXIS2_PLACEMENT_3D('',#20203,#15866,#15867);
#13115=AXIS2_PLACEMENT_3D('',#20205,#15868,#15869);
#13116=AXIS2_PLACEMENT_3D('',#20208,#15871,#15872);
#13117=AXIS2_PLACEMENT_3D('',#20209,#15873,#15874);
#13118=AXIS2_PLACEMENT_3D('',#20211,#15875,#15876);
#13119=AXIS2_PLACEMENT_3D('',#20212,#15877,#15878);
#13120=AXIS2_PLACEMENT_3D('',#20214,#15879,#15880);
#13121=AXIS2_PLACEMENT_3D('',#20215,#15881,#15882);
#13122=AXIS2_PLACEMENT_3D('',#20216,#15883,#15884);
#13123=AXIS2_PLACEMENT_3D('',#20218,#15886,#15887);
#13124=AXIS2_PLACEMENT_3D('',#20220,#15889,#15890);
#13125=AXIS2_PLACEMENT_3D('',#20224,#15893,#15894);
#13126=AXIS2_PLACEMENT_3D('',#20228,#15897,#15898);
#13127=AXIS2_PLACEMENT_3D('',#20230,#15900,#15901);
#13128=AXIS2_PLACEMENT_3D('',#20232,#15903,#15904);
#13129=AXIS2_PLACEMENT_3D('',#20233,#15905,#15906);
#13130=AXIS2_PLACEMENT_3D('',#20234,#15907,#15908);
#13131=AXIS2_PLACEMENT_3D('',#20235,#15909,#15910);
#13132=AXIS2_PLACEMENT_3D('',#20236,#15911,#15912);
#13133=AXIS2_PLACEMENT_3D('',#20237,#15913,#15914);
#13134=AXIS2_PLACEMENT_3D('',#20238,#15915,#15916);
#13135=AXIS2_PLACEMENT_3D('',#20330,#15919,#15920);
#13136=AXIS2_PLACEMENT_3D('',#20425,#15923,#15924);
#13137=AXIS2_PLACEMENT_3D('',#20426,#15925,#15926);
#13138=AXIS2_PLACEMENT_3D('',#20427,#15927,#15928);
#13139=AXIS2_PLACEMENT_3D('',#20428,#15929,#15930);
#13140=AXIS2_PLACEMENT_3D('',#20583,#15931,#15932);
#13141=AXIS2_PLACEMENT_3D('',#20638,#15933,#15934);
#13142=AXIS2_PLACEMENT_3D('',#20639,#15935,#15936);
#13143=AXIS2_PLACEMENT_3D('',#20767,#15937,#15938);
#13144=AXIS2_PLACEMENT_3D('',#20768,#15939,#15940);
#13145=AXIS2_PLACEMENT_3D('',#20769,#15941,#15942);
#13146=AXIS2_PLACEMENT_3D('',#20770,#15943,#15944);
#13147=AXIS2_PLACEMENT_3D('',#20771,#15945,#15946);
#13148=AXIS2_PLACEMENT_3D('',#20772,#15947,#15948);
#13149=AXIS2_PLACEMENT_3D('',#21012,#15949,#15950);
#13150=AXIS2_PLACEMENT_3D('',#21049,#15951,#15952);
#13151=AXIS2_PLACEMENT_3D('',#21116,#15953,#15954);
#13152=AXIS2_PLACEMENT_3D('',#21117,#15955,#15956);
#13153=AXIS2_PLACEMENT_3D('',#21118,#15957,#15958);
#13154=AXIS2_PLACEMENT_3D('',#21119,#15959,#15960);
#13155=AXIS2_PLACEMENT_3D('',#21120,#15961,#15962);
#13156=AXIS2_PLACEMENT_3D('',#21121,#15963,#15964);
#13157=AXIS2_PLACEMENT_3D('',#21122,#15965,#15966);
#13158=AXIS2_PLACEMENT_3D('',#21123,#15967,#15968);
#13159=AXIS2_PLACEMENT_3D('',#21124,#15969,#15970);
#13160=AXIS2_PLACEMENT_3D('',#21125,#15971,#15972);
#13161=AXIS2_PLACEMENT_3D('',#21126,#15973,#15974);
#13162=AXIS2_PLACEMENT_3D('',#21127,#15975,#15976);
#13163=AXIS2_PLACEMENT_3D('',#21128,#15977,#15978);
#13164=AXIS2_PLACEMENT_3D('',#21129,#15979,#15980);
#13165=AXIS2_PLACEMENT_3D('',#21130,#15981,#15982);
#13166=AXIS2_PLACEMENT_3D('',#21133,#15983,#15984);
#13167=AXIS2_PLACEMENT_3D('',#21146,#15985,#15986);
#13168=AXIS2_PLACEMENT_3D('',#21149,#15988,#15989);
#13169=AXIS2_PLACEMENT_3D('',#21151,#15990,#15991);
#13170=AXIS2_PLACEMENT_3D('',#21162,#15992,#15993);
#13171=AXIS2_PLACEMENT_3D('',#21182,#15995,#15996);
#13172=AXIS2_PLACEMENT_3D('',#21200,#15997,#15998);
#13173=AXIS2_PLACEMENT_3D('',#21202,#15999,#16000);
#13174=AXIS2_PLACEMENT_3D('',#21238,#16002,#16003);
#13175=AXIS2_PLACEMENT_3D('',#21241,#16004,#16005);
#13176=AXIS2_PLACEMENT_3D('',#21245,#16007,#16008);
#13177=AXIS2_PLACEMENT_3D('',#21246,#16009,#16010);
#13178=AXIS2_PLACEMENT_3D('',#21247,#16011,#16012);
#13179=AXIS2_PLACEMENT_3D('',#21248,#16013,#16014);
#13180=AXIS2_PLACEMENT_3D('',#21250,#16015,#16016);
#13181=AXIS2_PLACEMENT_3D('',#21252,#16018,#16019);
#13182=AXIS2_PLACEMENT_3D('',#21254,#16021,#16022);
#13183=AXIS2_PLACEMENT_3D('',#21255,#16023,#16024);
#13184=AXIS2_PLACEMENT_3D('',#21256,#16025,#16026);
#13185=AXIS2_PLACEMENT_3D('',#21257,#16027,#16028);
#13186=AXIS2_PLACEMENT_3D('',#21258,#16029,#16030);
#13187=AXIS2_PLACEMENT_3D('',#21259,#16031,#16032);
#13188=AXIS2_PLACEMENT_3D('',#21261,#16033,#16034);
#13189=AXIS2_PLACEMENT_3D('',#21264,#16036,#16037);
#13190=AXIS2_PLACEMENT_3D('',#21265,#16038,#16039);
#13191=AXIS2_PLACEMENT_3D('',#21267,#16040,#16041);
#13192=AXIS2_PLACEMENT_3D('',#21270,#16043,#16044);
#13193=AXIS2_PLACEMENT_3D('',#21271,#16045,#16046);
#13194=AXIS2_PLACEMENT_3D('',#21273,#16047,#16048);
#13195=AXIS2_PLACEMENT_3D('',#21276,#16050,#16051);
#13196=AXIS2_PLACEMENT_3D('',#21277,#16052,#16053);
#13197=AXIS2_PLACEMENT_3D('',#21279,#16054,#16055);
#13198=AXIS2_PLACEMENT_3D('',#21282,#16057,#16058);
#13199=AXIS2_PLACEMENT_3D('',#21283,#16059,#16060);
#13200=AXIS2_PLACEMENT_3D('',#21285,#16061,#16062);
#13201=AXIS2_PLACEMENT_3D('',#21288,#16064,#16065);
#13202=AXIS2_PLACEMENT_3D('',#21289,#16066,#16067);
#13203=AXIS2_PLACEMENT_3D('',#21290,#16068,#16069);
#13204=AXIS2_PLACEMENT_3D('',#21291,#16070,#16071);
#13205=AXIS2_PLACEMENT_3D('',#21292,#16072,#16073);
#13206=AXIS2_PLACEMENT_3D('',#21293,#16074,#16075);
#13207=AXIS2_PLACEMENT_3D('',#21294,#16076,#16077);
#13208=AXIS2_PLACEMENT_3D('',#21295,#16078,#16079);
#13209=AXIS2_PLACEMENT_3D('',#21296,#16080,#16081);
#13210=AXIS2_PLACEMENT_3D('',#21298,#16082,#16083);
#13211=AXIS2_PLACEMENT_3D('',#21299,#16084,#16085);
#13212=AXIS2_PLACEMENT_3D('',#21300,#16086,#16087);
#13213=AXIS2_PLACEMENT_3D('',#21301,#16088,#16089);
#13214=AXIS2_PLACEMENT_3D('',#21317,#16097,#16098);
#13215=AXIS2_PLACEMENT_3D('',#21318,#16099,#16100);
#13216=AXIS2_PLACEMENT_3D('',#21327,#16104,#16105);
#13217=AXIS2_PLACEMENT_3D('',#21335,#16110,#16111);
#13218=AXIS2_PLACEMENT_3D('',#21338,#16113,#16114);
#13219=AXIS2_PLACEMENT_3D('',#21342,#16116,#16117);
#13220=AXIS2_PLACEMENT_3D('',#21346,#16119,#16120);
#13221=AXIS2_PLACEMENT_3D('',#21350,#16122,#16123);
#13222=AXIS2_PLACEMENT_3D('',#21358,#16127,#16128);
#13223=AXIS2_PLACEMENT_3D('',#21362,#16130,#16131);
#13224=AXIS2_PLACEMENT_3D('',#21366,#16133,#16134);
#13225=AXIS2_PLACEMENT_3D('',#21369,#16136,#16137);
#13226=AXIS2_PLACEMENT_3D('',#21370,#16138,#16139);
#13227=AXIS2_PLACEMENT_3D('',#21379,#16143,#16144);
#13228=AXIS2_PLACEMENT_3D('',#21383,#16146,#16147);
#13229=AXIS2_PLACEMENT_3D('',#21387,#16149,#16150);
#13230=AXIS2_PLACEMENT_3D('',#21390,#16152,#16153);
#13231=AXIS2_PLACEMENT_3D('',#21393,#16155,#16156);
#13232=AXIS2_PLACEMENT_3D('',#21397,#16158,#16159);
#13233=AXIS2_PLACEMENT_3D('',#21401,#16161,#16162);
#13234=AXIS2_PLACEMENT_3D('',#21404,#16164,#16165);
#13235=AXIS2_PLACEMENT_3D('',#21405,#16166,#16167);
#13236=AXIS2_PLACEMENT_3D('',#21407,#16169,#16170);
#13237=AXIS2_PLACEMENT_3D('',#21409,#16172,#16173);
#13238=AXIS2_PLACEMENT_3D('',#21411,#16175,#16176);
#13239=AXIS2_PLACEMENT_3D('',#21413,#16178,#16179);
#13240=AXIS2_PLACEMENT_3D('',#21415,#16181,#16182);
#13241=AXIS2_PLACEMENT_3D('',#21417,#16184,#16185);
#13242=AXIS2_PLACEMENT_3D('',#21419,#16187,#16188);
#13243=AXIS2_PLACEMENT_3D('',#21425,#16191,#16192);
#13244=AXIS2_PLACEMENT_3D('',#21429,#16195,#16196);
#13245=AXIS2_PLACEMENT_3D('',#21431,#16198,#16199);
#13246=AXIS2_PLACEMENT_3D('',#21433,#16201,#16202);
#13247=AXIS2_PLACEMENT_3D('',#21435,#16204,#16205);
#13248=AXIS2_PLACEMENT_3D('',#21437,#16207,#16208);
#13249=AXIS2_PLACEMENT_3D('',#21439,#16210,#16211);
#13250=AXIS2_PLACEMENT_3D('',#21441,#16213,#16214);
#13251=AXIS2_PLACEMENT_3D('',#21443,#16216,#16217);
#13252=AXIS2_PLACEMENT_3D('',#21452,#16222,#16223);
#13253=AXIS2_PLACEMENT_3D('',#21453,#16224,#16225);
#13254=AXIS2_PLACEMENT_3D('',#21456,#16228,#16229);
#13255=AXIS2_PLACEMENT_3D('',#21458,#16231,#16232);
#13256=AXIS2_PLACEMENT_3D('',#21460,#16234,#16235);
#13257=AXIS2_PLACEMENT_3D('',#21463,#16238,#16239);
#13258=AXIS2_PLACEMENT_3D('',#21465,#16241,#16242);
#13259=AXIS2_PLACEMENT_3D('',#21467,#16244,#16245);
#13260=AXIS2_PLACEMENT_3D('',#21468,#16246,#16247);
#13261=AXIS2_PLACEMENT_3D('',#21469,#16248,#16249);
#13262=AXIS2_PLACEMENT_3D('',#21470,#16250,#16251);
#13263=AXIS2_PLACEMENT_3D('',#21471,#16252,#16253);
#13264=AXIS2_PLACEMENT_3D('',#21676,#16258,#16259);
#13265=AXIS2_PLACEMENT_3D('',#21754,#16261,#16262);
#13266=AXIS2_PLACEMENT_3D('',#21755,#16263,#16264);
#13267=AXIS2_PLACEMENT_3D('',#21758,#16266,#16267);
#13268=AXIS2_PLACEMENT_3D('',#21759,#16268,#16269);
#13269=AXIS2_PLACEMENT_3D('',#21760,#16270,#16271);
#13270=AXIS2_PLACEMENT_3D('',#21762,#16272,#16273);
#13271=AXIS2_PLACEMENT_3D('',#21810,#16275,#16276);
#13272=AXIS2_PLACEMENT_3D('',#21812,#16277,#16278);
#13273=AXIS2_PLACEMENT_3D('',#21813,#16279,#16280);
#13274=AXIS2_PLACEMENT_3D('',#21814,#16281,#16282);
#13275=AXIS2_PLACEMENT_3D('',#21817,#16283,#16284);
#13276=AXIS2_PLACEMENT_3D('',#21818,#16285,#16286);
#13277=AXIS2_PLACEMENT_3D('',#21821,#16288,#16289);
#13278=AXIS2_PLACEMENT_3D('',#21822,#16290,#16291);
#13279=AXIS2_PLACEMENT_3D('',#21825,#16293,#16294);
#13280=AXIS2_PLACEMENT_3D('',#21826,#16295,#16296);
#13281=AXIS2_PLACEMENT_3D('',#21827,#16297,#16298);
#13282=AXIS2_PLACEMENT_3D('',#21828,#16299,#16300);
#13283=AXIS2_PLACEMENT_3D('',#22105,#16305,#16306);
#13284=AXIS2_PLACEMENT_3D('',#22183,#16308,#16309);
#13285=AXIS2_PLACEMENT_3D('',#22184,#16310,#16311);
#13286=AXIS2_PLACEMENT_3D('',#22187,#16313,#16314);
#13287=AXIS2_PLACEMENT_3D('',#22188,#16315,#16316);
#13288=AXIS2_PLACEMENT_3D('',#22189,#16317,#16318);
#13289=AXIS2_PLACEMENT_3D('',#22191,#16319,#16320);
#13290=AXIS2_PLACEMENT_3D('',#22239,#16322,#16323);
#13291=AXIS2_PLACEMENT_3D('',#22241,#16324,#16325);
#13292=AXIS2_PLACEMENT_3D('',#22242,#16326,#16327);
#13293=AXIS2_PLACEMENT_3D('',#22243,#16328,#16329);
#13294=AXIS2_PLACEMENT_3D('',#22246,#16330,#16331);
#13295=AXIS2_PLACEMENT_3D('',#22247,#16332,#16333);
#13296=AXIS2_PLACEMENT_3D('',#22250,#16335,#16336);
#13297=AXIS2_PLACEMENT_3D('',#22251,#16337,#16338);
#13298=AXIS2_PLACEMENT_3D('',#22254,#16340,#16341);
#13299=AXIS2_PLACEMENT_3D('',#22255,#16342,#16343);
#13300=AXIS2_PLACEMENT_3D('',#22256,#16344,#16345);
#13301=AXIS2_PLACEMENT_3D('',#22257,#16346,#16347);
#13302=AXIS2_PLACEMENT_3D('',#22330,#16348,#16349);
#13303=AXIS2_PLACEMENT_3D('',#22331,#16350,#16351);
#13304=AXIS2_PLACEMENT_3D('',#22333,#16352,#16353);
#13305=AXIS2_PLACEMENT_3D('',#22335,#16354,#16355);
#13306=AXIS2_PLACEMENT_3D('',#22336,#16356,#16357);
#13307=AXIS2_PLACEMENT_3D('',#22337,#16358,#16359);
#13308=AXIS2_PLACEMENT_3D('',#22339,#16360,#16361);
#13309=AXIS2_PLACEMENT_3D('',#22341,#16362,#16363);
#13310=AXIS2_PLACEMENT_3D('',#22342,#16364,#16365);
#13311=AXIS2_PLACEMENT_3D('',#22343,#16366,#16367);
#13312=AXIS2_PLACEMENT_3D('',#22346,#16368,#16369);
#13313=AXIS2_PLACEMENT_3D('',#22347,#16370,#16371);
#13314=AXIS2_PLACEMENT_3D('',#22349,#16372,#16373);
#13315=AXIS2_PLACEMENT_3D('',#22350,#16374,#16375);
#13316=AXIS2_PLACEMENT_3D('',#22353,#16376,#16377);
#13317=AXIS2_PLACEMENT_3D('',#22354,#16378,#16379);
#13318=AXIS2_PLACEMENT_3D('',#22356,#16380,#16381);
#13319=AXIS2_PLACEMENT_3D('',#22357,#16382,#16383);
#13320=AXIS2_PLACEMENT_3D('',#22361,#16385,#16386);
#13321=AXIS2_PLACEMENT_3D('',#22362,#16387,#16388);
#13322=AXIS2_PLACEMENT_3D('',#22363,#16389,#16390);
#13323=AXIS2_PLACEMENT_3D('',#22365,#16391,#16392);
#13324=AXIS2_PLACEMENT_3D('',#22367,#16394,#16395);
#13325=AXIS2_PLACEMENT_3D('',#22368,#16396,#16397);
#13326=AXIS2_PLACEMENT_3D('',#22372,#16399,#16400);
#13327=AXIS2_PLACEMENT_3D('',#22373,#16401,#16402);
#13328=AXIS2_PLACEMENT_3D('',#22374,#16403,#16404);
#13329=AXIS2_PLACEMENT_3D('',#22376,#16405,#16406);
#13330=AXIS2_PLACEMENT_3D('',#22378,#16408,#16409);
#13331=AXIS2_PLACEMENT_3D('',#22379,#16410,#16411);
#13332=AXIS2_PLACEMENT_3D('',#22435,#16413,#16414);
#13333=AXIS2_PLACEMENT_3D('',#22437,#16415,#16416);
#13334=AXIS2_PLACEMENT_3D('',#22439,#16417,#16418);
#13335=AXIS2_PLACEMENT_3D('',#22440,#16419,#16420);
#13336=AXIS2_PLACEMENT_3D('',#22441,#16421,#16422);
#13337=AXIS2_PLACEMENT_3D('',#22443,#16423,#16424);
#13338=AXIS2_PLACEMENT_3D('',#22445,#16425,#16426);
#13339=AXIS2_PLACEMENT_3D('',#22446,#16427,#16428);
#13340=AXIS2_PLACEMENT_3D('',#22447,#16429,#16430);
#13341=AXIS2_PLACEMENT_3D('',#22450,#16431,#16432);
#13342=AXIS2_PLACEMENT_3D('',#22451,#16433,#16434);
#13343=AXIS2_PLACEMENT_3D('',#22453,#16435,#16436);
#13344=AXIS2_PLACEMENT_3D('',#22454,#16437,#16438);
#13345=AXIS2_PLACEMENT_3D('',#22457,#16439,#16440);
#13346=AXIS2_PLACEMENT_3D('',#22459,#16441,#16442);
#13347=AXIS2_PLACEMENT_3D('',#22460,#16443,#16444);
#13348=AXIS2_PLACEMENT_3D('',#22461,#16445,#16446);
#13349=AXIS2_PLACEMENT_3D('',#22465,#16448,#16449);
#13350=AXIS2_PLACEMENT_3D('',#22466,#16450,#16451);
#13351=AXIS2_PLACEMENT_3D('',#22467,#16452,#16453);
#13352=AXIS2_PLACEMENT_3D('',#22469,#16454,#16455);
#13353=AXIS2_PLACEMENT_3D('',#22471,#16457,#16458);
#13354=AXIS2_PLACEMENT_3D('',#22472,#16459,#16460);
#13355=AXIS2_PLACEMENT_3D('',#22476,#16462,#16463);
#13356=AXIS2_PLACEMENT_3D('',#22477,#16464,#16465);
#13357=AXIS2_PLACEMENT_3D('',#22478,#16466,#16467);
#13358=AXIS2_PLACEMENT_3D('',#22480,#16468,#16469);
#13359=AXIS2_PLACEMENT_3D('',#22482,#16471,#16472);
#13360=AXIS2_PLACEMENT_3D('',#22483,#16473,#16474);
#13361=AXIS2_PLACEMENT_3D('',#22539,#16476,#16477);
#13362=AXIS2_PLACEMENT_3D('',#22540,#16478,#16479);
#13363=AXIS2_PLACEMENT_3D('',#22541,#16480,#16481);
#13364=AXIS2_PLACEMENT_3D('',#22542,#16482,#16483);
#13365=AXIS2_PLACEMENT_3D('',#22543,#16484,#16485);
#13366=AXIS2_PLACEMENT_3D('',#22544,#16486,#16487);
#13367=AXIS2_PLACEMENT_3D('',#22545,#16488,#16489);
#13368=AXIS2_PLACEMENT_3D('',#22546,#16490,#16491);
#13369=AXIS2_PLACEMENT_3D('',#22547,#16492,#16493);
#13370=AXIS2_PLACEMENT_3D('',#22548,#16494,#16495);
#13371=AXIS2_PLACEMENT_3D('',#22550,#16496,#16497);
#13372=AXIS2_PLACEMENT_3D('',#22553,#16499,#16500);
#13373=AXIS2_PLACEMENT_3D('',#22554,#16501,#16502);
#13374=AXIS2_PLACEMENT_3D('',#22556,#16503,#16504);
#13375=AXIS2_PLACEMENT_3D('',#22559,#16506,#16507);
#13376=AXIS2_PLACEMENT_3D('',#22560,#16508,#16509);
#13377=AXIS2_PLACEMENT_3D('',#22562,#16510,#16511);
#13378=AXIS2_PLACEMENT_3D('',#22565,#16513,#16514);
#13379=AXIS2_PLACEMENT_3D('',#22566,#16515,#16516);
#13380=AXIS2_PLACEMENT_3D('',#22568,#16517,#16518);
#13381=AXIS2_PLACEMENT_3D('',#22571,#16520,#16521);
#13382=AXIS2_PLACEMENT_3D('',#22572,#16522,#16523);
#13383=AXIS2_PLACEMENT_3D('',#22574,#16524,#16525);
#13384=AXIS2_PLACEMENT_3D('',#22578,#16527,#16528);
#13385=AXIS2_PLACEMENT_3D('',#22582,#16530,#16531);
#13386=AXIS2_PLACEMENT_3D('',#22586,#16533,#16534);
#13387=AXIS2_PLACEMENT_3D('',#22590,#16536,#16537);
#13388=AXIS2_PLACEMENT_3D('',#22593,#16539,#16540);
#13389=AXIS2_PLACEMENT_3D('',#22594,#16541,#16542);
#13390=AXIS2_PLACEMENT_3D('',#22597,#16543,#16544);
#13391=AXIS2_PLACEMENT_3D('',#22615,#16546,#16547);
#13392=AXIS2_PLACEMENT_3D('',#22619,#16549,#16550);
#13393=AXIS2_PLACEMENT_3D('',#22621,#16551,#16552);
#13394=AXIS2_PLACEMENT_3D('',#22624,#16554,#16555);
#13395=AXIS2_PLACEMENT_3D('',#22626,#16556,#16557);
#13396=AXIS2_PLACEMENT_3D('',#22628,#16558,#16559);
#13397=AXIS2_PLACEMENT_3D('',#22632,#16561,#16562);
#13398=AXIS2_PLACEMENT_3D('',#22648,#16564,#16565);
#13399=AXIS2_PLACEMENT_3D('',#22655,#16570,#16571);
#13400=AXIS2_PLACEMENT_3D('',#22662,#16576,#16577);
#13401=AXIS2_PLACEMENT_3D('',#22665,#16580,#16581);
#13402=AXIS2_PLACEMENT_3D('',#22666,#16582,#16583);
#13403=AXIS2_PLACEMENT_3D('',#22672,#16587,#16588);
#13404=AXIS2_PLACEMENT_3D('',#22678,#16592,#16593);
#13405=AXIS2_PLACEMENT_3D('',#22684,#16597,#16598);
#13406=AXIS2_PLACEMENT_3D('',#22687,#16601,#16602);
#13407=AXIS2_PLACEMENT_3D('',#22688,#16603,#16604);
#13408=AXIS2_PLACEMENT_3D('',#22689,#16605,#16606);
#13409=AXIS2_PLACEMENT_3D('',#22695,#16610,#16611);
#13410=AXIS2_PLACEMENT_3D('',#22701,#16615,#16616);
#13411=AXIS2_PLACEMENT_3D('',#22707,#16620,#16621);
#13412=AXIS2_PLACEMENT_3D('',#22710,#16624,#16625);
#13413=AXIS2_PLACEMENT_3D('',#22711,#16626,#16627);
#13414=AXIS2_PLACEMENT_3D('',#22712,#16628,#16629);
#13415=AXIS2_PLACEMENT_3D('',#22713,#16630,#16631);
#13416=AXIS2_PLACEMENT_3D('',#22714,#16632,#16633);
#13417=AXIS2_PLACEMENT_3D('',#22715,#16634,#16635);
#13418=AXIS2_PLACEMENT_3D('',#22762,#16636,#16637);
#13419=AXIS2_PLACEMENT_3D('',#22763,#16638,#16639);
#13420=AXIS2_PLACEMENT_3D('',#22764,#16640,#16641);
#13421=AXIS2_PLACEMENT_3D('',#22765,#16642,#16643);
#13422=AXIS2_PLACEMENT_3D('',#23163,#16644,#16645);
#13423=AXIS2_PLACEMENT_3D('',#23164,#16646,#16647);
#13424=AXIS2_PLACEMENT_3D('',#23167,#16648,#16649);
#13425=AXIS2_PLACEMENT_3D('',#23168,#16650,#16651);
#13426=AXIS2_PLACEMENT_3D('',#23170,#16652,#16653);
#13427=AXIS2_PLACEMENT_3D('',#23172,#16654,#16655);
#13428=AXIS2_PLACEMENT_3D('',#23173,#16656,#16657);
#13429=AXIS2_PLACEMENT_3D('',#23174,#16658,#16659);
#13430=AXIS2_PLACEMENT_3D('',#23177,#16661,#16662);
#13431=AXIS2_PLACEMENT_3D('',#23178,#16663,#16664);
#13432=AXIS2_PLACEMENT_3D('',#23180,#16665,#16666);
#13433=AXIS2_PLACEMENT_3D('',#23182,#16668,#16669);
#13434=AXIS2_PLACEMENT_3D('',#23183,#16670,#16671);
#13435=AXIS2_PLACEMENT_3D('',#23184,#16672,#16673);
#13436=AXIS2_PLACEMENT_3D('',#23186,#16674,#16675);
#13437=AXIS2_PLACEMENT_3D('',#23188,#16676,#16677);
#13438=AXIS2_PLACEMENT_3D('',#23190,#16678,#16679);
#13439=AXIS2_PLACEMENT_3D('',#23191,#16680,#16681);
#13440=AXIS2_PLACEMENT_3D('',#23192,#16682,#16683);
#13441=AXIS2_PLACEMENT_3D('',#23195,#16684,#16685);
#13442=AXIS2_PLACEMENT_3D('',#23196,#16686,#16687);
#13443=AXIS2_PLACEMENT_3D('',#23198,#16688,#16689);
#13444=AXIS2_PLACEMENT_3D('',#23199,#16690,#16691);
#13445=AXIS2_PLACEMENT_3D('',#23200,#16692,#16693);
#13446=AXIS2_PLACEMENT_3D('',#23202,#16695,#16696);
#13447=AXIS2_PLACEMENT_3D('',#23204,#16697,#16698);
#13448=AXIS2_PLACEMENT_3D('',#23207,#16700,#16701);
#13449=AXIS2_PLACEMENT_3D('',#23208,#16702,#16703);
#13450=AXIS2_PLACEMENT_3D('',#23209,#16704,#16705);
#13451=AXIS2_PLACEMENT_3D('',#23210,#16706,#16707);
#13452=AXIS2_PLACEMENT_3D('',#23211,#16708,#16709);
#13453=AXIS2_PLACEMENT_3D('',#23212,#16710,#16711);
#13454=AXIS2_PLACEMENT_3D('',#23213,#16712,#16713);
#13455=AXIS2_PLACEMENT_3D('',#23214,#16714,#16715);
#13456=AXIS2_PLACEMENT_3D('',#23215,#16716,#16717);
#13457=AXIS2_PLACEMENT_3D('',#23216,#16718,#16719);
#13458=AXIS2_PLACEMENT_3D('',#23218,#16720,#16721);
#13459=AXIS2_PLACEMENT_3D('',#23221,#16723,#16724);
#13460=AXIS2_PLACEMENT_3D('',#23222,#16725,#16726);
#13461=AXIS2_PLACEMENT_3D('',#23225,#16727,#16728);
#13462=AXIS2_PLACEMENT_3D('',#23226,#16729,#16730);
#13463=AXIS2_PLACEMENT_3D('',#23229,#16732,#16733);
#13464=AXIS2_PLACEMENT_3D('',#23230,#16734,#16735);
#13465=AXIS2_PLACEMENT_3D('',#23232,#16737,#16738);
#13466=AXIS2_PLACEMENT_3D('',#23233,#16739,#16740);
#13467=AXIS2_PLACEMENT_3D('',#23234,#16741,#16742);
#13468=AXIS2_PLACEMENT_3D('',#23235,#16743,#16744);
#13469=AXIS2_PLACEMENT_3D('',#23238,#16745,#16746);
#13470=AXIS2_PLACEMENT_3D('',#23239,#16747,#16748);
#13471=AXIS2_PLACEMENT_3D('',#23242,#16750,#16751);
#13472=AXIS2_PLACEMENT_3D('',#23243,#16752,#16753);
#13473=AXIS2_PLACEMENT_3D('',#23245,#16754,#16755);
#13474=AXIS2_PLACEMENT_3D('',#23248,#16757,#16758);
#13475=AXIS2_PLACEMENT_3D('',#23249,#16759,#16760);
#13476=AXIS2_PLACEMENT_3D('',#23251,#16761,#16762);
#13477=AXIS2_PLACEMENT_3D('',#23253,#16763,#16764);
#13478=AXIS2_PLACEMENT_3D('',#23255,#16765,#16766);
#13479=AXIS2_PLACEMENT_3D('',#23256,#16767,#16768);
#13480=AXIS2_PLACEMENT_3D('',#23257,#16769,#16770);
#13481=AXIS2_PLACEMENT_3D('',#23259,#16771,#16772);
#13482=AXIS2_PLACEMENT_3D('',#23261,#16773,#16774);
#13483=AXIS2_PLACEMENT_3D('',#23262,#16775,#16776);
#13484=AXIS2_PLACEMENT_3D('',#23263,#16777,#16778);
#13485=AXIS2_PLACEMENT_3D('',#23266,#16779,#16780);
#13486=AXIS2_PLACEMENT_3D('',#23267,#16781,#16782);
#13487=AXIS2_PLACEMENT_3D('',#23269,#16783,#16784);
#13488=AXIS2_PLACEMENT_3D('',#23270,#16785,#16786);
#13489=AXIS2_PLACEMENT_3D('',#23271,#16787,#16788);
#13490=AXIS2_PLACEMENT_3D('',#23273,#16789,#16790);
#13491=AXIS2_PLACEMENT_3D('',#23275,#16791,#16792);
#13492=AXIS2_PLACEMENT_3D('',#23277,#16793,#16794);
#13493=AXIS2_PLACEMENT_3D('',#23278,#16795,#16796);
#13494=AXIS2_PLACEMENT_3D('',#23279,#16797,#16798);
#13495=AXIS2_PLACEMENT_3D('',#23281,#16799,#16800);
#13496=AXIS2_PLACEMENT_3D('',#23284,#16802,#16803);
#13497=AXIS2_PLACEMENT_3D('',#23285,#16804,#16805);
#13498=AXIS2_PLACEMENT_3D('',#23287,#16806,#16807);
#13499=AXIS2_PLACEMENT_3D('',#23290,#16809,#16810);
#13500=AXIS2_PLACEMENT_3D('',#23291,#16811,#16812);
#13501=AXIS2_PLACEMENT_3D('',#23293,#16814,#16815);
#13502=AXIS2_PLACEMENT_3D('',#23295,#16816,#16817);
#13503=AXIS2_PLACEMENT_3D('',#23298,#16819,#16820);
#13504=AXIS2_PLACEMENT_3D('',#23299,#16821,#16822);
#13505=AXIS2_PLACEMENT_3D('',#23301,#16824,#16825);
#13506=AXIS2_PLACEMENT_3D('',#23303,#16827,#16828);
#13507=AXIS2_PLACEMENT_3D('',#23304,#16829,#16830);
#13508=AXIS2_PLACEMENT_3D('',#23305,#16831,#16832);
#13509=AXIS2_PLACEMENT_3D('',#23306,#16833,#16834);
#13510=AXIS2_PLACEMENT_3D('',#23307,#16835,#16836);
#13511=AXIS2_PLACEMENT_3D('',#23308,#16837,#16838);
#13512=AXIS2_PLACEMENT_3D('',#23309,#16839,#16840);
#13513=AXIS2_PLACEMENT_3D('',#23310,#16841,#16842);
#13514=AXIS2_PLACEMENT_3D('',#23311,#16843,#16844);
#13515=AXIS2_PLACEMENT_3D('',#23312,#16845,#16846);
#13516=AXIS2_PLACEMENT_3D('',#23313,#16847,#16848);
#13517=AXIS2_PLACEMENT_3D('',#23316,#16849,#16850);
#13518=AXIS2_PLACEMENT_3D('',#23317,#16851,#16852);
#13519=AXIS2_PLACEMENT_3D('',#23320,#16854,#16855);
#13520=AXIS2_PLACEMENT_3D('',#23321,#16856,#16857);
#13521=AXIS2_PLACEMENT_3D('',#23323,#16858,#16859);
#13522=AXIS2_PLACEMENT_3D('',#23326,#16861,#16862);
#13523=AXIS2_PLACEMENT_3D('',#23327,#16863,#16864);
#13524=AXIS2_PLACEMENT_3D('',#23329,#16865,#16866);
#13525=AXIS2_PLACEMENT_3D('',#23331,#16867,#16868);
#13526=AXIS2_PLACEMENT_3D('',#23333,#16869,#16870);
#13527=AXIS2_PLACEMENT_3D('',#23334,#16871,#16872);
#13528=AXIS2_PLACEMENT_3D('',#23335,#16873,#16874);
#13529=AXIS2_PLACEMENT_3D('',#23337,#16875,#16876);
#13530=AXIS2_PLACEMENT_3D('',#23339,#16877,#16878);
#13531=AXIS2_PLACEMENT_3D('',#23340,#16879,#16880);
#13532=AXIS2_PLACEMENT_3D('',#23341,#16881,#16882);
#13533=AXIS2_PLACEMENT_3D('',#23344,#16883,#16884);
#13534=AXIS2_PLACEMENT_3D('',#23345,#16885,#16886);
#13535=AXIS2_PLACEMENT_3D('',#23347,#16887,#16888);
#13536=AXIS2_PLACEMENT_3D('',#23348,#16889,#16890);
#13537=AXIS2_PLACEMENT_3D('',#23349,#16891,#16892);
#13538=AXIS2_PLACEMENT_3D('',#23351,#16893,#16894);
#13539=AXIS2_PLACEMENT_3D('',#23353,#16895,#16896);
#13540=AXIS2_PLACEMENT_3D('',#23355,#16897,#16898);
#13541=AXIS2_PLACEMENT_3D('',#23356,#16899,#16900);
#13542=AXIS2_PLACEMENT_3D('',#23357,#16901,#16902);
#13543=AXIS2_PLACEMENT_3D('',#23359,#16903,#16904);
#13544=AXIS2_PLACEMENT_3D('',#23362,#16906,#16907);
#13545=AXIS2_PLACEMENT_3D('',#23363,#16908,#16909);
#13546=AXIS2_PLACEMENT_3D('',#23365,#16910,#16911);
#13547=AXIS2_PLACEMENT_3D('',#23368,#16913,#16914);
#13548=AXIS2_PLACEMENT_3D('',#23369,#16915,#16916);
#13549=AXIS2_PLACEMENT_3D('',#23371,#16918,#16919);
#13550=AXIS2_PLACEMENT_3D('',#23373,#16920,#16921);
#13551=AXIS2_PLACEMENT_3D('',#23376,#16923,#16924);
#13552=AXIS2_PLACEMENT_3D('',#23377,#16925,#16926);
#13553=AXIS2_PLACEMENT_3D('',#23379,#16928,#16929);
#13554=AXIS2_PLACEMENT_3D('',#23381,#16931,#16932);
#13555=AXIS2_PLACEMENT_3D('',#23382,#16933,#16934);
#13556=AXIS2_PLACEMENT_3D('',#23383,#16935,#16936);
#13557=AXIS2_PLACEMENT_3D('',#23384,#16937,#16938);
#13558=AXIS2_PLACEMENT_3D('',#23385,#16939,#16940);
#13559=AXIS2_PLACEMENT_3D('',#23386,#16941,#16942);
#13560=AXIS2_PLACEMENT_3D('',#23387,#16943,#16944);
#13561=AXIS2_PLACEMENT_3D('',#23389,#16945,#16946);
#13562=AXIS2_PLACEMENT_3D('',#23392,#16948,#16949);
#13563=AXIS2_PLACEMENT_3D('',#23393,#16950,#16951);
#13564=AXIS2_PLACEMENT_3D('',#23396,#16952,#16953);
#13565=AXIS2_PLACEMENT_3D('',#23397,#16954,#16955);
#13566=AXIS2_PLACEMENT_3D('',#23400,#16957,#16958);
#13567=AXIS2_PLACEMENT_3D('',#23401,#16959,#16960);
#13568=AXIS2_PLACEMENT_3D('',#23403,#16962,#16963);
#13569=AXIS2_PLACEMENT_3D('',#23404,#16964,#16965);
#13570=AXIS2_PLACEMENT_3D('',#23405,#16966,#16967);
#13571=AXIS2_PLACEMENT_3D('',#23430,#16970,#16971);
#13572=AXIS2_PLACEMENT_3D('',#23468,#16973,#16974);
#13573=AXIS2_PLACEMENT_3D('',#23506,#16976,#16977);
#13574=AXIS2_PLACEMENT_3D('',#23544,#16979,#16980);
#13575=AXIS2_PLACEMENT_3D('',#23582,#16982,#16983);
#13576=AXIS2_PLACEMENT_3D('',#23620,#16985,#16986);
#13577=AXIS2_PLACEMENT_3D('',#23658,#16988,#16989);
#13578=AXIS2_PLACEMENT_3D('',#23696,#16991,#16992);
#13579=AXIS2_PLACEMENT_3D('',#23734,#16994,#16995);
#13580=AXIS2_PLACEMENT_3D('',#23772,#16997,#16998);
#13581=AXIS2_PLACEMENT_3D('',#23810,#17000,#17001);
#13582=AXIS2_PLACEMENT_3D('',#23848,#17003,#17004);
#13583=AXIS2_PLACEMENT_3D('',#23886,#17006,#17007);
#13584=AXIS2_PLACEMENT_3D('',#23929,#17010,#17011);
#13585=AXIS2_PLACEMENT_3D('',#23989,#17013,#17014);
#13586=AXIS2_PLACEMENT_3D('',#24065,#17016,#17017);
#13587=AXIS2_PLACEMENT_3D('',#24143,#17019,#17020);
#13588=AXIS2_PLACEMENT_3D('',#24219,#17022,#17023);
#13589=AXIS2_PLACEMENT_3D('',#24295,#17025,#17026);
#13590=AXIS2_PLACEMENT_3D('',#24371,#17028,#17029);
#13591=AXIS2_PLACEMENT_3D('',#24447,#17031,#17032);
#13592=AXIS2_PLACEMENT_3D('',#24523,#17034,#17035);
#13593=AXIS2_PLACEMENT_3D('',#24601,#17037,#17038);
#13594=AXIS2_PLACEMENT_3D('',#24677,#17040,#17041);
#13595=AXIS2_PLACEMENT_3D('',#24753,#17043,#17044);
#13596=AXIS2_PLACEMENT_3D('',#24829,#17046,#17047);
#13597=AXIS2_PLACEMENT_3D('',#24844,#17048,#17049);
#13598=AXIS2_PLACEMENT_3D('',#24853,#17050,#17051);
#13599=AXIS2_PLACEMENT_3D('',#24855,#17052,#17053);
#13600=AXIS2_PLACEMENT_3D('',#24859,#17055,#17056);
#13601=AXIS2_PLACEMENT_3D('',#24861,#17057,#17058);
#13602=AXIS2_PLACEMENT_3D('',#24863,#17059,#17060);
#13603=AXIS2_PLACEMENT_3D('',#24864,#17061,#17062);
#13604=AXIS2_PLACEMENT_3D('',#24865,#17063,#17064);
#13605=AXIS2_PLACEMENT_3D('',#24867,#17065,#17066);
#13606=AXIS2_PLACEMENT_3D('',#24870,#17068,#17069);
#13607=AXIS2_PLACEMENT_3D('',#24871,#17070,#17071);
#13608=AXIS2_PLACEMENT_3D('',#24873,#17072,#17073);
#13609=AXIS2_PLACEMENT_3D('',#24876,#17075,#17076);
#13610=AXIS2_PLACEMENT_3D('',#24877,#17077,#17078);
#13611=AXIS2_PLACEMENT_3D('',#24893,#17080,#17081);
#13612=AXIS2_PLACEMENT_3D('',#24922,#17082,#17083);
#13613=AXIS2_PLACEMENT_3D('',#24935,#17084,#17085);
#13614=AXIS2_PLACEMENT_3D('',#24941,#17089,#17090);
#13615=AXIS2_PLACEMENT_3D('',#24945,#17093,#17094);
#13616=AXIS2_PLACEMENT_3D('',#24953,#17098,#17099);
#13617=AXIS2_PLACEMENT_3D('',#24954,#17100,#17101);
#13618=AXIS2_PLACEMENT_3D('',#24962,#17105,#17106);
#13619=AXIS2_PLACEMENT_3D('',#24963,#17107,#17108);
#13620=AXIS2_PLACEMENT_3D('',#24967,#17111,#17112);
#13621=AXIS2_PLACEMENT_3D('',#24975,#17116,#17117);
#13622=AXIS2_PLACEMENT_3D('',#24976,#17118,#17119);
#13623=AXIS2_PLACEMENT_3D('',#24984,#17123,#17124);
#13624=AXIS2_PLACEMENT_3D('',#24985,#17125,#17126);
#13625=AXIS2_PLACEMENT_3D('',#24994,#17131,#17132);
#13626=AXIS2_PLACEMENT_3D('',#24997,#17134,#17135);
#13627=AXIS2_PLACEMENT_3D('',#24999,#17136,#17137);
#13628=AXIS2_PLACEMENT_3D('',#25001,#17139,#17140);
#13629=AXIS2_PLACEMENT_3D('',#25003,#17141,#17142);
#13630=AXIS2_PLACEMENT_3D('',#25007,#17145,#17146);
#13631=AXIS2_PLACEMENT_3D('',#25008,#17147,#17148);
#13632=AXIS2_PLACEMENT_3D('',#25009,#17149,#17150);
#13633=AXIS2_PLACEMENT_3D('',#25010,#17151,#17152);
#13634=AXIS2_PLACEMENT_3D('',#25012,#17154,#17155);
#13635=AXIS2_PLACEMENT_3D('',#25013,#17156,#17157);
#13636=AXIS2_PLACEMENT_3D('',#25015,#17159,#17160);
#13637=AXIS2_PLACEMENT_3D('',#25016,#17161,#17162);
#13638=AXIS2_PLACEMENT_3D('',#25017,#17163,#17164);
#13639=AXIS2_PLACEMENT_3D('',#25020,#17167,#17168);
#13640=AXIS2_PLACEMENT_3D('',#25021,#17169,#17170);
#13641=AXIS2_PLACEMENT_3D('',#25022,#17171,#17172);
#13642=AXIS2_PLACEMENT_3D('',#25023,#17173,#17174);
#13643=AXIS2_PLACEMENT_3D('',#25024,#17175,#17176);
#13644=AXIS2_PLACEMENT_3D('',#25025,#17177,#17178);
#13645=AXIS2_PLACEMENT_3D('',#25026,#17179,#17180);
#13646=AXIS2_PLACEMENT_3D('',#25027,#17181,#17182);
#13647=AXIS2_PLACEMENT_3D('',#25028,#17183,#17184);
#13648=AXIS2_PLACEMENT_3D('',#25488,#17187,#17188);
#13649=AXIS2_PLACEMENT_3D('',#25950,#17189,#17190);
#13650=AXIS2_PLACEMENT_3D('',#25951,#17191,#17192);
#13651=AXIS2_PLACEMENT_3D('',#25952,#17193,#17194);
#13652=AXIS2_PLACEMENT_3D('',#25953,#17195,#17196);
#13653=AXIS2_PLACEMENT_3D('',#25954,#17197,#17198);
#13654=AXIS2_PLACEMENT_3D('',#25975,#17200,#17201);
#13655=AXIS2_PLACEMENT_3D('',#25993,#17202,#17203);
#13656=AXIS2_PLACEMENT_3D('',#26031,#17205,#17206);
#13657=AXIS2_PLACEMENT_3D('',#26069,#17208,#17209);
#13658=AXIS2_PLACEMENT_3D('',#26107,#17211,#17212);
#13659=AXIS2_PLACEMENT_3D('',#26145,#17214,#17215);
#13660=AXIS2_PLACEMENT_3D('',#26183,#17217,#17218);
#13661=AXIS2_PLACEMENT_3D('',#26221,#17220,#17221);
#13662=AXIS2_PLACEMENT_3D('',#26246,#17224,#17225);
#13663=AXIS2_PLACEMENT_3D('',#26294,#17229,#17230);
#13664=AXIS2_PLACEMENT_3D('',#26331,#17231,#17232);
#13665=AXIS2_PLACEMENT_3D('',#26409,#17234,#17235);
#13666=AXIS2_PLACEMENT_3D('',#26485,#17237,#17238);
#13667=AXIS2_PLACEMENT_3D('',#26561,#17240,#17241);
#13668=AXIS2_PLACEMENT_3D('',#26637,#17243,#17244);
#13669=AXIS2_PLACEMENT_3D('',#26713,#17246,#17247);
#13670=AXIS2_PLACEMENT_3D('',#26789,#17249,#17250);
#13671=AXIS2_PLACEMENT_3D('',#26807,#17252,#17253);
#13672=AXIS2_PLACEMENT_3D('',#26828,#17254,#17255);
#13673=AXIS2_PLACEMENT_3D('',#26901,#17256,#17257);
#13674=AXIS2_PLACEMENT_3D('',#26903,#17258,#17259);
#13675=AXIS2_PLACEMENT_3D('',#26906,#17261,#17262);
#13676=AXIS2_PLACEMENT_3D('',#26907,#17263,#17264);
#13677=AXIS2_PLACEMENT_3D('',#26960,#17277,#17278);
#13678=AXIS2_PLACEMENT_3D('',#26973,#17285,#17286);
#13679=AXIS2_PLACEMENT_3D('',#26974,#17287,#17288);
#13680=AXIS2_PLACEMENT_3D('',#26981,#17293,#17294);
#13681=AXIS2_PLACEMENT_3D('',#26986,#17298,#17299);
#13682=AXIS2_PLACEMENT_3D('',#26991,#17303,#17304);
#13683=AXIS2_PLACEMENT_3D('',#26996,#17308,#17309);
#13684=AXIS2_PLACEMENT_3D('',#27001,#17313,#17314);
#13685=AXIS2_PLACEMENT_3D('',#27004,#17317,#17318);
#13686=AXIS2_PLACEMENT_3D('',#27007,#17321,#17322);
#13687=AXIS2_PLACEMENT_3D('',#27686,#17323,#17324);
#13688=AXIS2_PLACEMENT_3D('',#27687,#17325,#17326);
#13689=AXIS2_PLACEMENT_3D('',#27688,#17327,#17328);
#13690=AXIS2_PLACEMENT_3D('',#27689,#17329,#17330);
#13691=AXIS2_PLACEMENT_3D('',#27690,#17331,#17332);
#13692=AXIS2_PLACEMENT_3D('',#27691,#17333,#17334);
#13693=AXIS2_PLACEMENT_3D('',#27692,#17335,#17336);
#13694=AXIS2_PLACEMENT_3D('',#27693,#17337,#17338);
#13695=AXIS2_PLACEMENT_3D('',#27695,#17339,#17340);
#13696=AXIS2_PLACEMENT_3D('',#27698,#17342,#17343);
#13697=AXIS2_PLACEMENT_3D('',#27699,#17344,#17345);
#13698=AXIS2_PLACEMENT_3D('',#27702,#17346,#17347);
#13699=AXIS2_PLACEMENT_3D('',#27703,#17348,#17349);
#13700=AXIS2_PLACEMENT_3D('',#27706,#17351,#17352);
#13701=AXIS2_PLACEMENT_3D('',#27707,#17353,#17354);
#13702=AXIS2_PLACEMENT_3D('',#27709,#17355,#17356);
#13703=AXIS2_PLACEMENT_3D('',#27711,#17358,#17359);
#13704=AXIS2_PLACEMENT_3D('',#27714,#17361,#17362);
#13705=AXIS2_PLACEMENT_3D('',#27715,#17363,#17364);
#13706=AXIS2_PLACEMENT_3D('',#27716,#17365,#17366);
#13707=AXIS2_PLACEMENT_3D('',#27717,#17367,#17368);
#13708=AXIS2_PLACEMENT_3D('',#27718,#17369,#17370);
#13709=AXIS2_PLACEMENT_3D('',#27719,#17371,#17372);
#13710=AXIS2_PLACEMENT_3D('',#27721,#17373,#17374);
#13711=AXIS2_PLACEMENT_3D('',#27724,#17376,#17377);
#13712=AXIS2_PLACEMENT_3D('',#27725,#17378,#17379);
#13713=AXIS2_PLACEMENT_3D('',#27728,#17380,#17381);
#13714=AXIS2_PLACEMENT_3D('',#27729,#17382,#17383);
#13715=AXIS2_PLACEMENT_3D('',#27732,#17385,#17386);
#13716=AXIS2_PLACEMENT_3D('',#27733,#17387,#17388);
#13717=AXIS2_PLACEMENT_3D('',#27735,#17390,#17391);
#13718=AXIS2_PLACEMENT_3D('',#27736,#17392,#17393);
#13719=AXIS2_PLACEMENT_3D('',#27737,#17394,#17395);
#13720=AXIS2_PLACEMENT_3D('',#27738,#17396,#17397);
#13721=AXIS2_PLACEMENT_3D('',#27739,#17398,#17399);
#13722=AXIS2_PLACEMENT_3D('',#27740,#17400,#17401);
#13723=AXIS2_PLACEMENT_3D('',#27741,#17402,#17403);
#13724=AXIS2_PLACEMENT_3D('',#27742,#17404,#17405);
#13725=AXIS2_PLACEMENT_3D('',#27743,#17406,#17407);
#13726=AXIS2_PLACEMENT_3D('',#27744,#17408,#17409);
#13727=AXIS2_PLACEMENT_3D('',#27745,#17410,#17411);
#13728=AXIS2_PLACEMENT_3D('',#27746,#17412,#17413);
#13729=AXIS2_PLACEMENT_3D('',#27747,#17414,#17415);
#13730=AXIS2_PLACEMENT_3D('',#27748,#17416,#17417);
#13731=AXIS2_PLACEMENT_3D('',#27749,#17418,#17419);
#13732=DIRECTION('axis',(0.,0.,1.));
#13733=DIRECTION('refdir',(1.,0.,0.));
#13734=DIRECTION('axis',(0.,0.,1.));
#13735=DIRECTION('refdir',(1.,0.,0.));
#13736=DIRECTION('center_axis',(0.,0.,-1.));
#13737=DIRECTION('ref_axis',(-1.,0.,0.));
#13738=DIRECTION('center_axis',(0.,0.,-1.));
#13739=DIRECTION('ref_axis',(1.,0.,0.));
#13740=DIRECTION('',(-0.707106781186543,8.65956056235488E-17,0.707106781186552));
#13741=DIRECTION('center_axis',(0.,0.,1.));
#13742=DIRECTION('ref_axis',(1.,0.,0.));
#13743=DIRECTION('center_axis',(0.,0.,1.));
#13744=DIRECTION('ref_axis',(1.,0.,0.));
#13745=DIRECTION('center_axis',(0.,0.,1.));
#13746=DIRECTION('ref_axis',(-1.,0.,0.));
#13747=DIRECTION('',(0.707106781186543,8.65956056235488E-17,-0.707106781186552));
#13748=DIRECTION('center_axis',(0.,0.,-1.));
#13749=DIRECTION('ref_axis',(-1.,0.,0.));
#13750=DIRECTION('center_axis',(0.,0.,-1.));
#13751=DIRECTION('ref_axis',(-1.,0.,0.));
#13752=DIRECTION('center_axis',(0.,0.,-1.));
#13753=DIRECTION('ref_axis',(1.,0.,0.));
#13754=DIRECTION('',(-0.707106781186552,8.65956056235498E-17,0.707106781186544));
#13755=DIRECTION('center_axis',(0.,0.,1.));
#13756=DIRECTION('ref_axis',(1.,0.,0.));
#13757=DIRECTION('center_axis',(0.,0.,-1.));
#13758=DIRECTION('ref_axis',(-1.,0.,0.));
#13759=DIRECTION('center_axis',(0.,0.,-1.));
#13760=DIRECTION('ref_axis',(1.,0.,0.));
#13761=DIRECTION('',(-0.70710678118656,8.65956056235508E-17,0.707106781186535));
#13762=DIRECTION('center_axis',(0.,0.,1.));
#13763=DIRECTION('ref_axis',(1.,0.,0.));
#13764=DIRECTION('center_axis',(0.,0.,1.));
#13765=DIRECTION('ref_axis',(1.,0.,0.));
#13766=DIRECTION('center_axis',(0.,0.,1.));
#13767=DIRECTION('ref_axis',(-1.,0.,0.));
#13768=DIRECTION('',(0.707106781186543,8.65956056235488E-17,-0.707106781186552));
#13769=DIRECTION('center_axis',(0.,0.,-1.));
#13770=DIRECTION('ref_axis',(-1.,0.,0.));
#13771=DIRECTION('center_axis',(0.,0.,1.));
#13772=DIRECTION('ref_axis',(1.,0.,0.));
#13773=DIRECTION('center_axis',(0.,0.,1.));
#13774=DIRECTION('ref_axis',(-1.,0.,0.));
#13775=DIRECTION('',(0.70710678118658,8.65956056235533E-17,-0.707106781186515));
#13776=DIRECTION('center_axis',(0.,0.,-1.));
#13777=DIRECTION('ref_axis',(-1.,0.,0.));
#13778=DIRECTION('center_axis',(-1.26920068081332E-33,-4.21788745889624E-34,
1.));
#13779=DIRECTION('ref_axis',(1.,-5.35334563442508E-67,1.26920068081332E-33));
#13780=DIRECTION('center_axis',(0.,0.,1.));
#13781=DIRECTION('ref_axis',(-1.,4.00913870003528E-14,0.));
#13782=DIRECTION('',(1.26920068081332E-33,4.21788745889624E-34,-1.));
#13783=DIRECTION('center_axis',(0.,0.,-1.));
#13784=DIRECTION('ref_axis',(-1.,0.,0.));
#13785=DIRECTION('',(8.7532076796714E-18,-2.63391976542839E-17,-1.));
#13786=DIRECTION('center_axis',(0.,-1.,0.));
#13787=DIRECTION('ref_axis',(0.,0.,-1.));
#13788=DIRECTION('center_axis',(0.,1.,0.));
#13789=DIRECTION('ref_axis',(0.,0.,-1.));
#13790=DIRECTION('center_axis',(0.12947657529132,-2.29349521067294E-15,
0.991582480911614));
#13791=DIRECTION('ref_axis',(0.991582480911614,5.32481111024183E-30,-0.12947657529132));
#13792=DIRECTION('center_axis',(0.,-1.,0.));
#13793=DIRECTION('ref_axis',(0.,0.,-1.));
#13794=DIRECTION('center_axis',(-2.31296463463574E-15,0.,-1.));
#13795=DIRECTION('ref_axis',(-1.,0.,2.31296463463574E-15));
#13796=DIRECTION('center_axis',(0.,0.,1.));
#13797=DIRECTION('ref_axis',(1.,0.,0.));
#13798=DIRECTION('center_axis',(0.,0.,1.));
#13799=DIRECTION('ref_axis',(1.,0.,0.));
#13800=DIRECTION('center_axis',(0.,1.,0.));
#13801=DIRECTION('ref_axis',(-1.,0.,0.));
#13802=DIRECTION('center_axis',(0.,0.,-1.));
#13803=DIRECTION('ref_axis',(1.,0.,0.));
#13804=DIRECTION('center_axis',(0.,0.,1.));
#13805=DIRECTION('ref_axis',(1.,0.,0.));
#13806=DIRECTION('center_axis',(0.,0.,1.));
#13807=DIRECTION('ref_axis',(1.,0.,0.));
#13808=DIRECTION('center_axis',(0.,1.,0.));
#13809=DIRECTION('ref_axis',(-1.,0.,0.));
#13810=DIRECTION('center_axis',(0.,0.,-1.));
#13811=DIRECTION('ref_axis',(1.,0.,0.));
#13812=DIRECTION('center_axis',(0.,0.,-1.));
#13813=DIRECTION('ref_axis',(-1.,0.,0.));
#13814=DIRECTION('center_axis',(0.,0.,-1.));
#13815=DIRECTION('ref_axis',(-1.,0.,0.));
#13816=DIRECTION('center_axis',(0.,1.,0.));
#13817=DIRECTION('ref_axis',(1.,0.,0.));
#13818=DIRECTION('center_axis',(0.,0.,1.));
#13819=DIRECTION('ref_axis',(-1.,0.,0.));
#13820=DIRECTION('center_axis',(0.,0.,-1.));
#13821=DIRECTION('ref_axis',(-1.,0.,0.));
#13822=DIRECTION('center_axis',(0.,0.,-1.));
#13823=DIRECTION('ref_axis',(-1.,0.,0.));
#13824=DIRECTION('center_axis',(0.,1.,0.));
#13825=DIRECTION('ref_axis',(1.,0.,0.));
#13826=DIRECTION('center_axis',(0.,0.,1.));
#13827=DIRECTION('ref_axis',(-1.,0.,0.));
#13828=DIRECTION('center_axis',(0.,0.,-1.));
#13829=DIRECTION('ref_axis',(-0.00404500334087533,-0.999991818940521,0.));
#13830=DIRECTION('center_axis',(0.,0.,-1.));
#13831=DIRECTION('ref_axis',(-1.,0.,0.));
#13832=DIRECTION('center_axis',(0.960335432337036,-0.27884737294448,-7.73956934497999E-15));
#13833=DIRECTION('ref_axis',(0.27884737294448,0.960335432337036,3.94430452610506E-31));
#13834=DIRECTION('center_axis',(0.,0.,1.));
#13835=DIRECTION('ref_axis',(-1.,0.,0.));
#13836=DIRECTION('center_axis',(0.,0.,1.));
#13837=DIRECTION('ref_axis',(-1.,0.,0.));
#13838=DIRECTION('center_axis',(-0.962559864875271,-0.271069191409314,0.));
#13839=DIRECTION('ref_axis',(0.271069191409314,-0.962559864875271,0.));
#13840=DIRECTION('center_axis',(0.,0.,1.));
#13841=DIRECTION('ref_axis',(-0.00404500334087533,-0.999991818940521,0.));
#13842=DIRECTION('center_axis',(0.,0.,1.));
#13843=DIRECTION('ref_axis',(1.,0.,0.));
#13844=DIRECTION('center_axis',(-0.96255986487527,-0.271069191409318,3.76184071961435E-15));
#13845=DIRECTION('ref_axis',(0.271069191409318,-0.96255986487527,0.));
#13846=DIRECTION('center_axis',(0.,0.,-1.));
#13847=DIRECTION('ref_axis',(1.,0.,0.));
#13848=DIRECTION('center_axis',(0.,0.,-1.));
#13849=DIRECTION('ref_axis',(1.,0.,0.));
#13850=DIRECTION('center_axis',(0.960335432337038,-0.278847372944473,0.));
#13851=DIRECTION('ref_axis',(0.278847372944473,0.960335432337038,0.));
#13852=DIRECTION('center_axis',(0.,0.,1.));
#13853=DIRECTION('ref_axis',(1.,0.,0.));
#13854=DIRECTION('center_axis',(0.,0.,1.));
#13855=DIRECTION('ref_axis',(1.,0.,0.));
#13856=DIRECTION('center_axis',(0.,1.,0.));
#13857=DIRECTION('ref_axis',(-1.,0.,0.));
#13858=DIRECTION('center_axis',(0.,0.,-1.));
#13859=DIRECTION('ref_axis',(1.,0.,0.));
#13860=DIRECTION('center_axis',(0.,0.,-1.));
#13861=DIRECTION('ref_axis',(1.,0.,0.));
#13862=DIRECTION('center_axis',(0.,0.,-1.));
#13863=DIRECTION('ref_axis',(-1.,0.,0.));
#13864=DIRECTION('center_axis',(0.,0.,-1.));
#13865=DIRECTION('ref_axis',(-1.,0.,0.));
#13866=DIRECTION('center_axis',(0.,1.,0.));
#13867=DIRECTION('ref_axis',(1.,0.,0.));
#13868=DIRECTION('center_axis',(0.,0.,1.));
#13869=DIRECTION('ref_axis',(-1.,0.,0.));
#13870=DIRECTION('center_axis',(0.,0.,1.));
#13871=DIRECTION('ref_axis',(1.,0.,0.));
#13872=DIRECTION('center_axis',(0.,0.,1.));
#13873=DIRECTION('ref_axis',(1.,0.,0.));
#13874=DIRECTION('center_axis',(0.,0.,1.));
#13875=DIRECTION('ref_axis',(1.,0.,0.));
#13876=DIRECTION('center_axis',(0.,1.,0.));
#13877=DIRECTION('ref_axis',(-1.,0.,0.));
#13878=DIRECTION('center_axis',(0.,0.,-1.));
#13879=DIRECTION('ref_axis',(1.,0.,0.));
#13880=DIRECTION('center_axis',(0.,0.,-1.));
#13881=DIRECTION('ref_axis',(-1.,0.,0.));
#13882=DIRECTION('center_axis',(0.,0.,-1.));
#13883=DIRECTION('ref_axis',(-1.,0.,0.));
#13884=DIRECTION('center_axis',(0.,0.,-1.));
#13885=DIRECTION('ref_axis',(-1.,0.,0.));
#13886=DIRECTION('center_axis',(0.,1.,0.));
#13887=DIRECTION('ref_axis',(1.,0.,0.));
#13888=DIRECTION('center_axis',(0.,0.,1.));
#13889=DIRECTION('ref_axis',(-1.,0.,0.));
#13890=DIRECTION('center_axis',(0.,1.,0.));
#13891=DIRECTION('ref_axis',(0.,0.,1.));
#13892=DIRECTION('center_axis',(0.,1.,3.85494105772624E-16));
#13893=DIRECTION('ref_axis',(0.,-3.85494105772624E-16,1.));
#13894=DIRECTION('',(0.,-1.,0.));
#13895=DIRECTION('center_axis',(0.,-1.,0.));
#13896=DIRECTION('ref_axis',(0.,0.,-1.));
#13897=DIRECTION('center_axis',(-0.0915537643933219,0.707106781186538,-0.70115469635839));
#13898=DIRECTION('ref_axis',(0.091553764391814,0.707106781186557,0.701154696358567));
#13899=DIRECTION('',(0.,1.,0.));
#13900=DIRECTION('center_axis',(0.,1.,0.));
#13901=DIRECTION('ref_axis',(0.,0.,-1.));
#13902=DIRECTION('center_axis',(0.,-1.,0.));
#13903=DIRECTION('ref_axis',(0.,0.,-1.));
#13904=DIRECTION('center_axis',(0.,-1.,0.));
#13905=DIRECTION('ref_axis',(0.,0.,-1.));
#13906=DIRECTION('center_axis',(0.,0.,1.));
#13907=DIRECTION('ref_axis',(1.,0.,0.));
#13908=DIRECTION('center_axis',(0.,1.,0.));
#13909=DIRECTION('ref_axis',(1.02798428206033E-15,0.,-1.));
#13910=DIRECTION('center_axis',(-0.129476575291326,0.,-0.991582480911613));
#13911=DIRECTION('ref_axis',(-0.991582480911613,0.,0.129476575291326));
#13912=DIRECTION('center_axis',(0.,0.,1.));
#13913=DIRECTION('ref_axis',(1.,0.,0.));
#13914=DIRECTION('center_axis',(0.,0.,-1.));
#13915=DIRECTION('ref_axis',(-1.,0.,0.));
#13916=DIRECTION('',(0.,0.,1.));
#13917=DIRECTION('center_axis',(0.,0.,1.));
#13918=DIRECTION('ref_axis',(1.,0.,0.));
#13919=DIRECTION('center_axis',(0.,0.,-1.));
#13920=DIRECTION('ref_axis',(-1.,0.,0.));
#13921=DIRECTION('',(0.,0.,1.));
#13922=DIRECTION('center_axis',(0.,0.,-1.));
#13923=DIRECTION('ref_axis',(-1.,0.,0.));
#13924=DIRECTION('',(0.,0.,1.));
#13925=DIRECTION('center_axis',(0.,0.,-1.));
#13926=DIRECTION('ref_axis',(-1.,0.,0.));
#13927=DIRECTION('',(0.,0.,1.));
#13928=DIRECTION('center_axis',(0.,-1.,0.));
#13929=DIRECTION('ref_axis',(0.,0.,-1.));
#13930=DIRECTION('',(0.,-1.,0.));
#13931=DIRECTION('center_axis',(-8.08177633281312E-16,0.958646866278096,
0.284598288426311));
#13932=DIRECTION('ref_axis',(1.40325551131645E-13,-0.284598288426311,0.958646866278096));
#13933=DIRECTION('',(0.,-1.,0.));
#13934=DIRECTION('center_axis',(0.,0.,1.));
#13935=DIRECTION('ref_axis',(1.,0.,0.));
#13936=DIRECTION('',(0.,0.,-1.));
#13937=DIRECTION('center_axis',(0.,0.,1.));
#13938=DIRECTION('ref_axis',(1.,0.,0.));
#13939=DIRECTION('center_axis',(0.,0.,1.));
#13940=DIRECTION('ref_axis',(1.,0.,0.));
#13941=DIRECTION('center_axis',(0.,0.,1.));
#13942=DIRECTION('ref_axis',(1.,0.,0.));
#13943=DIRECTION('',(0.,0.,1.));
#13944=DIRECTION('center_axis',(0.,0.,-1.));
#13945=DIRECTION('ref_axis',(-1.,0.,0.));
#13946=DIRECTION('center_axis',(0.,0.,1.));
#13947=DIRECTION('ref_axis',(1.,0.,0.));
#13948=DIRECTION('center_axis',(0.,0.,1.));
#13949=DIRECTION('ref_axis',(1.,0.,0.));
#13950=DIRECTION('',(0.,0.,1.));
#13951=DIRECTION('center_axis',(0.,0.,-1.));
#13952=DIRECTION('ref_axis',(-1.,0.,0.));
#13953=DIRECTION('center_axis',(0.,0.,1.));
#13954=DIRECTION('ref_axis',(1.,0.,0.));
#13955=DIRECTION('center_axis',(0.,0.,1.));
#13956=DIRECTION('ref_axis',(1.,0.,0.));
#13957=DIRECTION('',(0.,0.,1.));
#13958=DIRECTION('center_axis',(0.,0.,-1.));
#13959=DIRECTION('ref_axis',(-1.,0.,0.));
#13960=DIRECTION('center_axis',(0.,0.,1.));
#13961=DIRECTION('ref_axis',(1.,0.,0.));
#13962=DIRECTION('',(0.,0.,-1.));
#13963=DIRECTION('center_axis',(0.,0.,1.));
#13964=DIRECTION('ref_axis',(1.,0.,0.));
#13965=DIRECTION('',(0.,0.,-1.));
#13966=DIRECTION('center_axis',(0.,0.,1.));
#13967=DIRECTION('ref_axis',(1.,0.,0.));
#13968=DIRECTION('',(0.,0.,-1.));
#13969=DIRECTION('center_axis',(0.,0.,-1.));
#13970=DIRECTION('ref_axis',(-1.,0.,0.));
#13971=DIRECTION('',(0.,0.,1.));
#13972=DIRECTION('center_axis',(0.,0.,1.));
#13973=DIRECTION('ref_axis',(1.,0.,0.));
#13974=DIRECTION('center_axis',(0.,0.,-1.));
#13975=DIRECTION('ref_axis',(-1.,0.,0.));
#13976=DIRECTION('center_axis',(0.,0.,1.));
#13977=DIRECTION('ref_axis',(1.,0.,0.));
#13978=DIRECTION('',(0.,0.,-1.));
#13979=DIRECTION('center_axis',(0.,0.,-1.));
#13980=DIRECTION('ref_axis',(-1.,0.,0.));
#13981=DIRECTION('center_axis',(0.,0.,-1.));
#13982=DIRECTION('ref_axis',(-1.,0.,0.));
#13983=DIRECTION('center_axis',(0.,0.,1.));
#13984=DIRECTION('ref_axis',(1.,0.,0.));
#13985=DIRECTION('',(0.,0.,-1.));
#13986=DIRECTION('center_axis',(0.,0.,-1.));
#13987=DIRECTION('ref_axis',(-1.,0.,0.));
#13988=DIRECTION('center_axis',(0.,0.,-1.));
#13989=DIRECTION('ref_axis',(-1.,0.,0.));
#13990=DIRECTION('center_axis',(0.,0.,1.));
#13991=DIRECTION('ref_axis',(1.,0.,0.));
#13992=DIRECTION('',(0.,0.,-1.));
#13993=DIRECTION('center_axis',(0.,0.,-1.));
#13994=DIRECTION('ref_axis',(-1.,0.,0.));
#13995=DIRECTION('center_axis',(0.,0.,-1.));
#13996=DIRECTION('ref_axis',(-1.,0.,0.));
#13997=DIRECTION('',(0.,0.,1.));
#13998=DIRECTION('center_axis',(0.,-1.,0.));
#13999=DIRECTION('ref_axis',(0.,0.,-1.));
#14000=DIRECTION('center_axis',(0.,-1.,0.));
#14001=DIRECTION('ref_axis',(0.,0.,-1.));
#14002=DIRECTION('',(0.,-1.,0.));
#14003=DIRECTION('center_axis',(0.,1.,0.));
#14004=DIRECTION('ref_axis',(0.,0.,-1.));
#14005=DIRECTION('center_axis',(0.,-1.,0.));
#14006=DIRECTION('ref_axis',(0.,0.,-1.));
#14007=DIRECTION('',(0.,-1.,0.));
#14008=DIRECTION('center_axis',(-2.75380126257971E-15,0.958646866278097,
0.284598288426308));
#14009=DIRECTION('ref_axis',(1.36429802923528E-12,-0.284598288426308,0.958646866278097));
#14010=DIRECTION('',(0.,-1.,0.));
#14011=DIRECTION('center_axis',(0.,-1.,0.));
#14012=DIRECTION('ref_axis',(0.,0.,-1.));
#14013=DIRECTION('center_axis',(0.,1.,0.));
#14014=DIRECTION('ref_axis',(0.,0.,1.));
#14015=DIRECTION('',(0.,-1.,0.));
#14016=DIRECTION('center_axis',(0.,-1.,0.));
#14017=DIRECTION('ref_axis',(0.,0.,-1.));
#14018=DIRECTION('center_axis',(0.,-1.,0.));
#14019=DIRECTION('ref_axis',(0.,0.,-1.));
#14020=DIRECTION('',(2.52323414687536E-15,0.,1.));
#14021=DIRECTION('',(1.,0.,0.));
#14022=DIRECTION('',(0.,0.,1.));
#14023=DIRECTION('center_axis',(0.,1.,0.));
#14024=DIRECTION('ref_axis',(0.,0.,-1.));
#14025=DIRECTION('',(1.,0.,0.));
#14026=DIRECTION('center_axis',(0.,-1.,0.));
#14027=DIRECTION('ref_axis',(0.,0.,-1.));
#14028=DIRECTION('',(1.,0.,0.));
#14029=DIRECTION('',(0.,0.,1.));
#14030=DIRECTION('',(1.,0.,0.));
#14031=DIRECTION('',(0.,0.,-1.));
#14032=DIRECTION('center_axis',(0.,-1.,0.));
#14033=DIRECTION('ref_axis',(0.,0.,-1.));
#14034=DIRECTION('',(-0.129476575291326,0.,-0.991582480911613));
#14035=DIRECTION('',(1.,0.,0.));
#14036=DIRECTION('',(-0.129476575291322,0.,-0.991582480911614));
#14037=DIRECTION('',(1.,0.,0.));
#14038=DIRECTION('center_axis',(0.,1.,0.));
#14039=DIRECTION('ref_axis',(0.,0.,1.));
#14040=DIRECTION('',(0.,0.,-1.));
#14041=DIRECTION('',(-1.,0.,0.));
#14042=DIRECTION('',(2.52323414687536E-15,0.,-1.));
#14043=DIRECTION('',(1.,0.,0.));
#14044=DIRECTION('center_axis',(0.,1.,0.));
#14045=DIRECTION('ref_axis',(0.,0.,1.));
#14046=DIRECTION('center_axis',(0.,1.,0.));
#14047=DIRECTION('ref_axis',(0.,0.,1.));
#14048=DIRECTION('',(1.,0.,0.));
#14049=DIRECTION('',(0.,0.,1.));
#14050=DIRECTION('',(1.,0.,0.));
#14051=DIRECTION('',(0.,0.,-1.));
#14052=DIRECTION('center_axis',(0.,1.,0.));
#14053=DIRECTION('ref_axis',(0.,0.,1.));
#14054=DIRECTION('',(-0.129476575291322,0.,0.991582480911614));
#14055=DIRECTION('',(-1.,0.,0.));
#14056=DIRECTION('',(-0.129476575291321,0.,0.991582480911614));
#14057=DIRECTION('center_axis',(0.,1.,0.));
#14058=DIRECTION('ref_axis',(0.,0.,1.));
#14059=DIRECTION('',(1.,0.,0.));
#14060=DIRECTION('center_axis',(0.,0.,1.));
#14061=DIRECTION('ref_axis',(1.,0.,0.));
#14062=DIRECTION('center_axis',(-0.671022843491604,-0.222998528050286,0.707106781186441));
#14063=DIRECTION('ref_axis',(0.671022846456233,0.222998519128768,0.707106781186654));
#14064=DIRECTION('',(0.,0.,1.));
#14065=DIRECTION('center_axis',(0.,0.,1.));
#14066=DIRECTION('ref_axis',(-1.,0.,0.));
#14067=DIRECTION('center_axis',(0.,0.,1.));
#14068=DIRECTION('ref_axis',(-1.,3.91353616180368E-14,0.));
#14069=DIRECTION('center_axis',(0.,0.,1.));
#14070=DIRECTION('ref_axis',(-1.,-1.06858966120171E-14,0.));
#14071=DIRECTION('',(0.,0.,1.));
#14072=DIRECTION('center_axis',(0.,0.,-1.));
#14073=DIRECTION('ref_axis',(-1.,0.,0.));
#14074=DIRECTION('center_axis',(-0.315367542755717,0.948969605928568,-2.77555756156289E-17));
#14075=DIRECTION('ref_axis',(-0.948969605928567,-0.315367542755717,0.));
#14076=DIRECTION('',(0.671022843492016,0.222998528048706,0.707106781186547));
#14077=DIRECTION('',(-0.948969605928567,-0.315367542755717,0.));
#14078=DIRECTION('',(0.671022843492016,0.222998528048706,-0.707106781186548));
#14079=DIRECTION('center_axis',(0.315367542755717,-0.948969605928567,2.77555756156289E-17));
#14080=DIRECTION('ref_axis',(-0.948969605928567,-0.315367542755717,3.08148791101958E-33));
#14081=DIRECTION('',(0.948969605928567,0.315367542755717,5.68761795402233E-17));
#14082=DIRECTION('center_axis',(0.315367542755717,-0.948969605928567,2.77555756156289E-17));
#14083=DIRECTION('ref_axis',(-0.948969605928567,-0.315367542755718,1.57107031786579E-15));
#14084=DIRECTION('center_axis',(0.,-1.,0.));
#14085=DIRECTION('ref_axis',(0.,0.,-1.));
#14086=DIRECTION('',(1.,0.,0.));
#14087=DIRECTION('',(0.,0.,-1.));
#14088=DIRECTION('',(1.,0.,0.));
#14089=DIRECTION('',(0.,0.,1.));
#14090=DIRECTION('center_axis',(0.,-0.958646866278097,-0.28459828842631));
#14091=DIRECTION('ref_axis',(0.,0.28459828842631,-0.958646866278097));
#14092=DIRECTION('',(0.,-0.28459828842631,0.958646866278097));
#14093=DIRECTION('',(1.,0.,0.));
#14094=DIRECTION('',(2.41889050778795E-15,-0.28459828842631,0.958646866278097));
#14095=DIRECTION('',(-0.124206667879909,0.28239446456039,-0.95122345957184));
#14096=DIRECTION('',(1.,0.,0.));
#14097=DIRECTION('',(-0.124206667879913,0.28239446456039,-0.95122345957184));
#14098=DIRECTION('center_axis',(1.,0.,0.));
#14099=DIRECTION('ref_axis',(0.,0.,-1.));
#14100=DIRECTION('center_axis',(1.,0.,0.));
#14101=DIRECTION('ref_axis',(0.,0.,-1.));
#14102=DIRECTION('',(1.,0.,0.));
#14103=DIRECTION('center_axis',(1.,0.,-2.52323414687536E-15));
#14104=DIRECTION('ref_axis',(-2.52323414687536E-15,0.,-1.));
#14105=DIRECTION('center_axis',(1.,0.,0.));
#14106=DIRECTION('ref_axis',(0.,0.,-1.));
#14107=DIRECTION('',(1.,0.,0.));
#14108=DIRECTION('center_axis',(-0.991582480911615,3.94488230498385E-15,
0.129476575291316));
#14109=DIRECTION('ref_axis',(0.129476575291316,-1.79884483303906E-11,0.991582480911614));
#14110=DIRECTION('center_axis',(-0.991582480911611,3.9101256326932E-16,
0.12947657529134));
#14111=DIRECTION('ref_axis',(0.12947657529134,-8.50893575937157E-12,0.991582480911611));
#14112=DIRECTION('center_axis',(0.,0.,-1.));
#14113=DIRECTION('ref_axis',(-1.,0.,0.));
#14114=DIRECTION('',(0.,-1.,0.));
#14115=DIRECTION('',(-1.,0.,0.));
#14116=DIRECTION('',(0.,-1.,0.));
#14117=DIRECTION('center_axis',(0.,0.,-1.));
#14118=DIRECTION('ref_axis',(-1.,0.,0.));
#14119=DIRECTION('',(0.,1.,0.));
#14120=DIRECTION('',(-1.,0.,0.));
#14121=DIRECTION('',(0.,1.,0.));
#14122=DIRECTION('center_axis',(1.,0.,-2.52323414687536E-15));
#14123=DIRECTION('ref_axis',(-2.52323414687536E-15,0.,-1.));
#14124=DIRECTION('',(0.,-1.,0.));
#14125=DIRECTION('',(-2.52323414687536E-15,0.,-1.));
#14126=DIRECTION('center_axis',(-1.,0.,2.52323414687536E-15));
#14127=DIRECTION('ref_axis',(-2.52323414687536E-15,0.,-1.));
#14128=DIRECTION('center_axis',(-0.991582480911614,0.,0.129476575291322));
#14129=DIRECTION('ref_axis',(0.129476575291322,0.,0.991582480911614));
#14130=DIRECTION('',(0.129476575291322,0.,0.991582480911614));
#14131=DIRECTION('',(0.,-1.,0.));
#14132=DIRECTION('center_axis',(0.991582480911629,9.22717350759991E-14,
-0.129476575291207));
#14133=DIRECTION('ref_axis',(0.129476575291207,3.62398433939346E-12,0.991582480911629));
#14134=DIRECTION('center_axis',(0.,0.,-1.));
#14135=DIRECTION('ref_axis',(1.,0.,0.));
#14136=DIRECTION('center_axis',(0.,0.,1.));
#14137=DIRECTION('ref_axis',(-1.,-1.38777878078144E-14,0.));
#14138=DIRECTION('',(-1.,0.,0.));
#14139=DIRECTION('center_axis',(0.,0.,1.));
#14140=DIRECTION('ref_axis',(-1.,-1.38777878078144E-14,0.));
#14141=DIRECTION('center_axis',(0.,0.,-1.));
#14142=DIRECTION('ref_axis',(-1.,0.,0.));
#14143=DIRECTION('',(0.,-1.,0.));
#14144=DIRECTION('center_axis',(0.,0.,-1.));
#14145=DIRECTION('ref_axis',(-1.,0.,0.));
#14146=DIRECTION('',(-0.948969605928567,-0.315367542755717,0.));
#14147=DIRECTION('',(0.315367542755717,-0.948969605928567,0.));
#14148=DIRECTION('',(0.948969605928568,0.315367542755717,0.));
#14149=DIRECTION('',(-0.946881588720454,0.32158242635789,0.));
#14150=DIRECTION('center_axis',(0.,0.,-1.));
#14151=DIRECTION('ref_axis',(-1.,0.,0.));
#14152=DIRECTION('',(0.,1.,0.));
#14153=DIRECTION('center_axis',(0.,0.,-1.));
#14154=DIRECTION('ref_axis',(-1.,0.,0.));
#14155=DIRECTION('',(1.,0.,0.));
#14156=DIRECTION('center_axis',(0.,0.,1.));
#14157=DIRECTION('ref_axis',(-1.,0.,0.));
#14158=DIRECTION('',(1.,0.,0.));
#14159=DIRECTION('center_axis',(0.,0.,1.));
#14160=DIRECTION('ref_axis',(1.,-3.92466554034205E-11,0.));
#14161=DIRECTION('center_axis',(0.,0.,1.));
#14162=DIRECTION('ref_axis',(1.,0.,0.));
#14163=DIRECTION('',(1.,0.,0.));
#14164=DIRECTION('center_axis',(0.,0.,1.));
#14165=DIRECTION('ref_axis',(1.,0.,0.));
#14166=DIRECTION('',(-1.,0.,0.));
#14167=DIRECTION('center_axis',(0.,0.,1.));
#14168=DIRECTION('ref_axis',(1.,0.,0.));
#14169=DIRECTION('center_axis',(0.,0.,-1.));
#14170=DIRECTION('ref_axis',(1.,0.,0.));
#14171=DIRECTION('',(0.,-1.,0.));
#14172=DIRECTION('center_axis',(0.,0.,-1.));
#14173=DIRECTION('ref_axis',(1.,1.85037170770859E-15,0.));
#14174=DIRECTION('',(-0.948969605928567,-0.315367542755717,0.));
#14175=DIRECTION('center_axis',(0.,0.,1.));
#14176=DIRECTION('ref_axis',(1.,0.,0.));
#14177=DIRECTION('',(0.948969605928567,0.315367542755717,0.));
#14178=DIRECTION('center_axis',(0.,0.,1.));
#14179=DIRECTION('ref_axis',(1.,0.,0.));
#14180=DIRECTION('center_axis',(0.,0.,-1.));
#14181=DIRECTION('ref_axis',(1.,0.,0.));
#14182=DIRECTION('center_axis',(0.,0.,-1.));
#14183=DIRECTION('ref_axis',(1.,3.60822483003176E-15,0.));
#14184=DIRECTION('',(-0.946881588720454,0.32158242635789,0.));
#14185=DIRECTION('center_axis',(0.,0.,-1.));
#14186=DIRECTION('ref_axis',(1.,9.25185853854296E-16,0.));
#14187=DIRECTION('',(0.,1.,0.));
#14188=DIRECTION('center_axis',(0.,0.,-1.));
#14189=DIRECTION('ref_axis',(1.,0.,0.));
#14190=DIRECTION('center_axis',(0.315367542755717,-0.948969605928568,0.));
#14191=DIRECTION('ref_axis',(0.948969605928567,0.315367542755717,0.));
#14192=DIRECTION('',(-0.948969605928567,-0.315367542755717,0.));
#14193=DIRECTION('',(-1.26920068081332E-33,-4.21788745889624E-34,-1.));
#14194=DIRECTION('',(0.,0.,1.));
#14195=DIRECTION('center_axis',(0.,0.,-1.));
#14196=DIRECTION('ref_axis',(-1.,0.,0.));
#14197=DIRECTION('',(0.,1.,0.));
#14198=DIRECTION('',(1.,0.,0.));
#14199=DIRECTION('',(0.,1.,0.));
#14200=DIRECTION('',(1.,0.,0.));
#14201=DIRECTION('center_axis',(1.,0.,0.));
#14202=DIRECTION('ref_axis',(0.,0.,-1.));
#14203=DIRECTION('center_axis',(1.,0.,0.));
#14204=DIRECTION('ref_axis',(0.,6.93889390390722E-16,1.));
#14205=DIRECTION('',(1.,0.,0.));
#14206=DIRECTION('center_axis',(1.,0.,2.52323414687536E-15));
#14207=DIRECTION('ref_axis',(-2.52323414687536E-15,0.,1.));
#14208=DIRECTION('center_axis',(0.,0.,1.));
#14209=DIRECTION('ref_axis',(1.,0.,0.));
#14210=DIRECTION('center_axis',(0.,0.,-1.));
#14211=DIRECTION('ref_axis',(1.,-1.38777878078144E-14,0.));
#14212=DIRECTION('',(1.,0.,0.));
#14213=DIRECTION('center_axis',(0.,0.,-1.));
#14214=DIRECTION('ref_axis',(1.,-1.38777878078144E-14,0.));
#14215=DIRECTION('',(1.,0.,0.));
#14216=DIRECTION('center_axis',(0.,0.,1.));
#14217=DIRECTION('ref_axis',(1.,0.,0.));
#14218=DIRECTION('',(0.,1.,0.));
#14219=DIRECTION('center_axis',(0.,0.,1.));
#14220=DIRECTION('ref_axis',(1.,0.,0.));
#14221=DIRECTION('',(-0.946881588720454,0.32158242635789,0.));
#14222=DIRECTION('center_axis',(0.,0.,1.));
#14223=DIRECTION('ref_axis',(1.,0.,0.));
#14224=DIRECTION('',(-0.948969605928568,-0.315367542755717,0.));
#14225=DIRECTION('',(-0.315367542755717,0.948969605928567,0.));
#14226=DIRECTION('center_axis',(0.,0.,-1.));
#14227=DIRECTION('ref_axis',(1.,1.54197642309049E-14,0.));
#14228=DIRECTION('center_axis',(0.,0.,1.));
#14229=DIRECTION('ref_axis',(1.,0.,0.));
#14230=DIRECTION('',(0.,-1.,0.));
#14231=DIRECTION('center_axis',(0.,0.,1.));
#14232=DIRECTION('ref_axis',(1.,0.,0.));
#14233=DIRECTION('',(0.,-1.,0.));
#14234=DIRECTION('center_axis',(0.,0.,-1.));
#14235=DIRECTION('ref_axis',(1.,0.,0.));
#14236=DIRECTION('',(1.,0.,0.));
#14237=DIRECTION('center_axis',(0.,0.,-1.));
#14238=DIRECTION('ref_axis',(1.,-5.03906675906735E-11,0.));
#14239=DIRECTION('',(0.,-1.,0.));
#14240=DIRECTION('',(1.,0.,0.));
#14241=DIRECTION('center_axis',(1.,0.,0.));
#14242=DIRECTION('ref_axis',(0.,0.,-1.));
#14243=DIRECTION('',(0.,0.,1.));
#14244=DIRECTION('',(0.,0.,-1.));
#14245=DIRECTION('center_axis',(0.,1.,0.));
#14246=DIRECTION('ref_axis',(0.,0.,1.));
#14247=DIRECTION('',(0.,0.,-1.));
#14248=DIRECTION('',(0.,0.,1.));
#14249=DIRECTION('center_axis',(-1.,0.,0.));
#14250=DIRECTION('ref_axis',(0.,0.,1.));
#14251=DIRECTION('',(0.,0.,-1.));
#14252=DIRECTION('',(0.,0.,1.));
#14253=DIRECTION('center_axis',(-0.32158242635789,-0.946881588720455,0.));
#14254=DIRECTION('ref_axis',(0.946881588720455,-0.32158242635789,0.));
#14255=DIRECTION('',(0.,0.,-1.));
#14256=DIRECTION('',(0.,0.,1.));
#14257=DIRECTION('center_axis',(0.,0.,1.));
#14258=DIRECTION('ref_axis',(1.,0.,0.));
#14259=DIRECTION('center_axis',(-1.,0.,-2.52323414687536E-15));
#14260=DIRECTION('ref_axis',(-2.52323414687536E-15,0.,1.));
#14261=DIRECTION('',(0.,-1.,0.));
#14262=DIRECTION('',(2.52323414687536E-15,0.,-1.));
#14263=DIRECTION('center_axis',(-1.,0.,-2.52323414687536E-15));
#14264=DIRECTION('ref_axis',(-2.52323414687536E-15,0.,1.));
#14265=DIRECTION('',(-2.41889050778795E-15,0.28459828842631,0.958646866278097));
#14266=DIRECTION('center_axis',(0.,-1.,0.));
#14267=DIRECTION('ref_axis',(-0.0648749531344179,0.,0.997893401348965));
#14268=DIRECTION('',(0.,-1.,0.));
#14269=DIRECTION('center_axis',(0.,-1.,0.));
#14270=DIRECTION('ref_axis',(0.,0.,-1.));
#14271=DIRECTION('center_axis',(-1.96841463568603E-16,0.958646866278096,
-0.284598288426311));
#14272=DIRECTION('ref_axis',(6.29350215176821E-14,0.284598288426311,0.958646866278096));
#14273=DIRECTION('center_axis',(0.991582480911614,0.,0.129476575291322));
#14274=DIRECTION('ref_axis',(0.129476575291322,0.,-0.991582480911614));
#14275=DIRECTION('',(-0.129476575291322,0.,0.991582480911614));
#14276=DIRECTION('',(0.124206667879909,-0.28239446456039,-0.95122345957184));
#14277=DIRECTION('center_axis',(-0.991582480911612,3.71896393509484E-15,
-0.129476575291335));
#14278=DIRECTION('ref_axis',(0.129476575291335,-1.65123794436265E-11,-0.991582480911612));
#14279=DIRECTION('',(0.,-1.,0.));
#14280=DIRECTION('center_axis',(0.991582480911607,-7.77925334389506E-14,
0.129476575291374));
#14281=DIRECTION('ref_axis',(0.129476575291374,-9.20853362991702E-11,-0.991582480911607));
#14282=DIRECTION('center_axis',(0.,-1.,0.));
#14283=DIRECTION('ref_axis',(0.,0.,-1.));
#14284=DIRECTION('center_axis',(0.,1.,0.));
#14285=DIRECTION('ref_axis',(0.,0.,-1.));
#14286=DIRECTION('',(0.129476575291322,0.,-0.991582480911614));
#14287=DIRECTION('',(-2.52323414687536E-15,0.,1.));
#14288=DIRECTION('center_axis',(0.,0.,-1.));
#14289=DIRECTION('ref_axis',(-1.,0.,0.));
#14290=DIRECTION('',(0.,-1.,0.));
#14291=DIRECTION('',(1.,0.,0.));
#14292=DIRECTION('',(1.,0.,0.));
#14293=DIRECTION('center_axis',(1.,0.,0.));
#14294=DIRECTION('ref_axis',(0.,0.,-1.));
#14295=DIRECTION('',(1.,0.,0.));
#14296=DIRECTION('center_axis',(-0.991582480911613,7.99403462683938E-16,
-0.129476575291326));
#14297=DIRECTION('ref_axis',(0.129476575291326,-1.62736358106788E-11,-0.991582480911613));
#14298=DIRECTION('center_axis',(0.,0.958646866278097,-0.28459828842631));
#14299=DIRECTION('ref_axis',(0.,0.28459828842631,0.958646866278097));
#14300=DIRECTION('',(0.,0.28459828842631,0.958646866278097));
#14301=DIRECTION('center_axis',(-5.40194110194962E-16,0.958646866278097,
-0.28459828842631));
#14302=DIRECTION('ref_axis',(-5.49346011511301E-14,0.28459828842631,0.958646866278097));
#14303=DIRECTION('',(0.124206667879908,-0.28239446456039,-0.95122345957184));
#14304=DIRECTION('center_axis',(0.,-1.,0.));
#14305=DIRECTION('ref_axis',(0.,0.,-1.));
#14306=DIRECTION('',(-0.129476575291321,0.,0.991582480911614));
#14307=DIRECTION('center_axis',(0.,-1.,0.));
#14308=DIRECTION('ref_axis',(0.,0.,-1.));
#14309=DIRECTION('',(0.,0.,-1.));
#14310=DIRECTION('',(0.99997906305609,0.,-0.00647096974680808));
#14311=DIRECTION('center_axis',(-1.,0.,0.));
#14312=DIRECTION('ref_axis',(0.,0.,1.));
#14313=DIRECTION('center_axis',(1.,0.,0.));
#14314=DIRECTION('ref_axis',(0.,0.,1.));
#14315=DIRECTION('',(0.,1.,0.));
#14316=DIRECTION('',(0.,0.,1.));
#14317=DIRECTION('',(0.,-1.,0.));
#14318=DIRECTION('center_axis',(0.,-1.,0.));
#14319=DIRECTION('ref_axis',(-0.0648749531344181,0.,0.997893401348965));
#14320=DIRECTION('center_axis',(0.,1.,0.));
#14321=DIRECTION('ref_axis',(0.,0.,-1.));
#14322=DIRECTION('',(0.,-1.,0.));
#14323=DIRECTION('center_axis',(0.991582480911614,0.,0.129476575291321));
#14324=DIRECTION('ref_axis',(0.129476575291321,0.,-0.991582480911614));
#14325=DIRECTION('center_axis',(-0.991582480911602,-5.10163316335803E-15,
-0.129476575291414));
#14326=DIRECTION('ref_axis',(0.129476575291414,-9.29749157779182E-11,-0.991582480911602));
#14327=DIRECTION('',(0.129476575291321,0.,-0.991582480911614));
#14328=DIRECTION('',(0.,-1.,0.));
#14329=DIRECTION('center_axis',(-0.00647096974680808,0.,-0.99997906305609));
#14330=DIRECTION('ref_axis',(-0.99997906305609,0.,0.00647096974680808));
#14331=DIRECTION('',(0.99997906305609,0.,-0.00647096974680808));
#14332=DIRECTION('',(0.,1.,0.));
#14333=DIRECTION('',(-0.99997906305609,0.,0.00647096974680808));
#14334=DIRECTION('',(0.,-1.,0.));
#14335=DIRECTION('center_axis',(0.,0.,-1.));
#14336=DIRECTION('ref_axis',(-1.,0.,0.));
#14337=DIRECTION('',(0.,0.,1.));
#14338=DIRECTION('center_axis',(0.671022843491264,0.222998528051552,0.707106781186364));
#14339=DIRECTION('ref_axis',(0.671022847566698,0.222998515787032,-0.707106781186732));
#14340=DIRECTION('center_axis',(0.,0.,-1.));
#14341=DIRECTION('ref_axis',(1.,2.48412401759879E-14,0.));
#14342=DIRECTION('center_axis',(0.,0.,-1.));
#14343=DIRECTION('ref_axis',(-1.,0.,0.));
#14344=DIRECTION('center_axis',(0.,0.,-1.));
#14345=DIRECTION('ref_axis',(-1.,0.,0.));
#14346=DIRECTION('center_axis',(0.,0.,-1.));
#14347=DIRECTION('ref_axis',(-1.,0.,0.));
#14348=DIRECTION('center_axis',(0.,0.,-1.));
#14349=DIRECTION('ref_axis',(-1.,0.,0.));
#14350=DIRECTION('center_axis',(-5.39737656850081E-17,-1.79369009829332E-17,
-1.));
#14351=DIRECTION('ref_axis',(-1.,0.,5.39737656850081E-17));
#14352=DIRECTION('',(0.948969605928567,0.315367542755717,-5.68761795402233E-17));
#14353=DIRECTION('',(0.315367542755717,-0.948969605928567,0.));
#14354=DIRECTION('',(0.948969605928567,0.315367542755717,-5.68761795402233E-17));
#14355=DIRECTION('',(-0.315367542755717,0.948969605928567,3.08148791101958E-33));
#14356=DIRECTION('center_axis',(-0.315367542755717,0.948969605928568,2.77555756156289E-17));
#14357=DIRECTION('ref_axis',(-0.948969605928567,-0.315367542755717,0.));
#14358=DIRECTION('',(0.671022843492016,0.222998528048706,0.707106781186548));
#14359=DIRECTION('',(0.948969605928567,0.315367542755717,0.));
#14360=DIRECTION('',(0.671022843492016,0.222998528048706,-0.707106781186547));
#14361=DIRECTION('center_axis',(0.315367542755717,-0.948969605928567,-2.77555756156289E-17));
#14362=DIRECTION('ref_axis',(-0.948969605928567,-0.315367542755718,1.54074395550979E-33));
#14363=DIRECTION('center_axis',(0.315367542755717,-0.948969605928567,-2.77555756156289E-17));
#14364=DIRECTION('ref_axis',(-0.948969605928567,-0.315367542755718,2.09476042382105E-15));
#14365=DIRECTION('center_axis',(0.671022843492016,0.222998528048706,-0.707106781186547));
#14366=DIRECTION('ref_axis',(-0.725372545860843,-1.38777878078145E-17,-0.688356498996966));
#14367=DIRECTION('',(0.671022843492016,0.222998528048706,0.707106781186548));
#14368=DIRECTION('center_axis',(0.671022843492036,0.222998528048696,-0.707106781186532));
#14369=DIRECTION('ref_axis',(0.671022843491931,0.222998528048912,0.707106781186563));
#14370=DIRECTION('',(-0.315367542755717,0.948969605928567,-9.8130778667736E-18));
#14371=DIRECTION('center_axis',(-0.948969605928568,-0.315367542755717,1.33745135026891E-33));
#14372=DIRECTION('ref_axis',(0.315367542755717,-0.948969605928567,0.));
#14373=DIRECTION('',(0.315367542755717,-0.948969605928567,0.));
#14374=DIRECTION('',(-1.26920068081332E-33,-4.21788745889624E-34,-1.));
#14375=DIRECTION('center_axis',(0.948969605928568,0.315367542755717,-1.33745135026891E-33));
#14376=DIRECTION('ref_axis',(0.315367542755717,-0.948969605928567,1.38777878078145E-14));
#14377=DIRECTION('',(-8.7532076796714E-18,2.63391976542839E-17,-1.));
#14378=DIRECTION('center_axis',(-0.671022843492015,-0.222998528048706,-0.707106781186548));
#14379=DIRECTION('ref_axis',(-0.725372545860843,-2.77555756156289E-17,0.688356498996965));
#14380=DIRECTION('',(0.671022843492016,0.222998528048706,-0.707106781186547));
#14381=DIRECTION('',(0.315367542755717,-0.948969605928567,-2.65650496374544E-17));
#14382=DIRECTION('center_axis',(-0.671022843492001,-0.222998528048843,-0.707106781186518));
#14383=DIRECTION('ref_axis',(0.671022843489952,0.222998528054823,-0.707106781186577));
#14384=DIRECTION('center_axis',(-0.671022843492014,-0.222998528048677,-0.707106781186559));
#14385=DIRECTION('ref_axis',(0.671022843491969,0.222998528048881,-0.707106781186537));
#14386=DIRECTION('center_axis',(-0.315367542755717,0.948969605928568,2.77555756156289E-17));
#14387=DIRECTION('ref_axis',(-0.948969605928567,-0.315367542755717,0.));
#14388=DIRECTION('',(-0.948969605928567,-0.315367542755717,0.));
#14389=DIRECTION('',(8.7532076796714E-18,-2.63391976542839E-17,1.));
#14390=DIRECTION('center_axis',(-0.315367542755717,0.948969605928567,2.77555756156289E-17));
#14391=DIRECTION('ref_axis',(-0.948969605928568,-0.315367542755717,7.70371977754894E-33));
#14392=DIRECTION('center_axis',(-0.315367542755717,0.948969605928567,2.77555756156289E-17));
#14393=DIRECTION('ref_axis',(-0.948969605928567,-0.315367542755718,1.54074395550979E-33));
#14394=DIRECTION('center_axis',(0.,0.,-1.));
#14395=DIRECTION('ref_axis',(-1.,0.,0.));
#14396=DIRECTION('center_axis',(0.,0.,-1.));
#14397=DIRECTION('ref_axis',(-1.,0.,0.));
#14398=DIRECTION('center_axis',(0.,0.,-1.));
#14399=DIRECTION('ref_axis',(-1.,0.,0.));
#14400=DIRECTION('center_axis',(-1.,0.,0.));
#14401=DIRECTION('ref_axis',(0.,0.,1.));
#14402=DIRECTION('',(0.,0.,1.));
#14403=DIRECTION('',(0.,-1.,0.));
#14404=DIRECTION('',(0.,0.,-1.));
#14405=DIRECTION('center_axis',(-0.315367542755717,0.948969605928568,0.));
#14406=DIRECTION('ref_axis',(-0.948969605928567,-0.315367542755717,0.));
#14407=DIRECTION('',(-0.948969605928567,-0.315367542755717,0.));
#14408=DIRECTION('',(0.,0.,1.));
#14409=DIRECTION('center_axis',(0.32158242635789,0.946881588720455,0.));
#14410=DIRECTION('ref_axis',(-0.946881588720455,0.32158242635789,0.));
#14411=DIRECTION('',(-0.946881588720454,0.32158242635789,0.));
#14412=DIRECTION('',(0.,0.,-1.));
#14413=DIRECTION('center_axis',(1.,0.,0.));
#14414=DIRECTION('ref_axis',(0.,0.,-1.));
#14415=DIRECTION('',(0.,1.,0.));
#14416=DIRECTION('',(0.,0.,-1.));
#14417=DIRECTION('',(0.,0.,1.));
#14418=DIRECTION('center_axis',(0.,0.,-1.));
#14419=DIRECTION('ref_axis',(1.,0.,0.));
#14420=DIRECTION('center_axis',(0.,0.,-1.));
#14421=DIRECTION('ref_axis',(-1.,0.,0.));
#14422=DIRECTION('',(1.,0.,0.));
#14423=DIRECTION('center_axis',(0.,0.,-1.));
#14424=DIRECTION('ref_axis',(-1.,0.,0.));
#14425=DIRECTION('center_axis',(0.,0.,1.));
#14426=DIRECTION('ref_axis',(-1.,0.,0.));
#14427=DIRECTION('center_axis',(0.,0.,1.));
#14428=DIRECTION('ref_axis',(-1.,0.,0.));
#14429=DIRECTION('center_axis',(0.,0.,-1.));
#14430=DIRECTION('ref_axis',(-1.,0.,0.));
#14431=DIRECTION('',(-0.948969605928567,-0.315367542755717,0.));
#14432=DIRECTION('center_axis',(0.,0.,1.));
#14433=DIRECTION('ref_axis',(-1.,-9.25185853854296E-16,0.));
#14434=DIRECTION('center_axis',(0.,0.,1.));
#14435=DIRECTION('ref_axis',(-1.,0.,0.));
#14436=DIRECTION('center_axis',(0.,0.,-1.));
#14437=DIRECTION('ref_axis',(1.,0.,0.));
#14438=DIRECTION('center_axis',(0.,-1.,0.));
#14439=DIRECTION('ref_axis',(0.,0.,1.));
#14440=DIRECTION('',(-0.129476575291322,0.,-0.991582480911614));
#14441=DIRECTION('',(2.52323414687536E-15,0.,1.));
#14442=DIRECTION('center_axis',(0.00647096974680808,0.,-0.99997906305609));
#14443=DIRECTION('ref_axis',(-0.99997906305609,0.,-0.00647096974680808));
#14444=DIRECTION('',(-0.99997906305609,0.,-0.00647096974680808));
#14445=DIRECTION('',(0.99997906305609,0.,0.00647096974680808));
#14446=DIRECTION('',(0.,1.,0.));
#14447=DIRECTION('center_axis',(0.00647096974627404,-2.69158824529299E-10,
-0.999979063056094));
#14448=DIRECTION('ref_axis',(-0.00333013267216393,0.999994454860619,-2.1549908119201E-5));
#14449=DIRECTION('center_axis',(1.,0.,0.));
#14450=DIRECTION('ref_axis',(0.,0.,-1.));
#14451=DIRECTION('center_axis',(1.,0.,0.));
#14452=DIRECTION('ref_axis',(0.,0.,-1.));
#14453=DIRECTION('',(0.,0.,1.));
#14454=DIRECTION('',(0.,-1.,0.));
#14455=DIRECTION('center_axis',(-0.991582480911613,0.,0.129476575291326));
#14456=DIRECTION('ref_axis',(0.129476575291326,0.,0.991582480911613));
#14457=DIRECTION('center_axis',(-0.991582480911623,-1.21982113180531E-13,
0.129476575291247));
#14458=DIRECTION('ref_axis',(0.129476575291247,3.37745991995288E-11,0.991582480911624));
#14459=DIRECTION('',(-0.129476575291326,0.,-0.991582480911613));
#14460=DIRECTION('center_axis',(0.,-1.,0.));
#14461=DIRECTION('ref_axis',(0.,0.,-1.));
#14462=DIRECTION('',(0.129476575291326,0.,0.991582480911613));
#14463=DIRECTION('',(0.,0.,-1.));
#14464=DIRECTION('center_axis',(0.,0.,1.));
#14465=DIRECTION('ref_axis',(1.,0.,0.));
#14466=DIRECTION('center_axis',(0.,0.,1.));
#14467=DIRECTION('ref_axis',(1.,0.,0.));
#14468=DIRECTION('center_axis',(0.,0.,1.));
#14469=DIRECTION('ref_axis',(1.,0.,0.));
#14470=DIRECTION('center_axis',(0.,0.,1.));
#14471=DIRECTION('ref_axis',(1.,0.,0.));
#14472=DIRECTION('center_axis',(0.948969605928568,0.315367542755717,1.33745135026891E-33));
#14473=DIRECTION('ref_axis',(-0.315367542755717,0.948969605928567,0.));
#14474=DIRECTION('center_axis',(0.948969605928568,0.315367542755717,1.33745135026891E-33));
#14475=DIRECTION('ref_axis',(-0.315367542755717,0.948969605928567,1.28292706084425E-48));
#14476=DIRECTION('',(1.26920068081332E-33,4.21788745889624E-34,-1.));
#14477=DIRECTION('',(0.315367542755717,-0.948969605928567,0.));
#14478=DIRECTION('',(-8.7532076796714E-18,2.63391976542839E-17,1.));
#14479=DIRECTION('center_axis',(0.671022843492015,0.222998528048706,-0.707106781186548));
#14480=DIRECTION('ref_axis',(-0.725372545860843,-2.77555756156289E-17,-0.688356498996965));
#14481=DIRECTION('',(-0.315367542755717,0.948969605928567,-2.65650496374544E-17));
#14482=DIRECTION('',(0.671022843492016,0.222998528048706,0.707106781186547));
#14483=DIRECTION('center_axis',(-0.671022843492013,-0.222998528048675,0.70710678118656));
#14484=DIRECTION('ref_axis',(0.671022843492034,0.22299852804869,0.707106781186535));
#14485=DIRECTION('center_axis',(-0.671022843491897,-0.222998528049469,0.70710678118642));
#14486=DIRECTION('ref_axis',(0.671022843488484,0.222998528058928,0.707106781186675));
#14487=DIRECTION('center_axis',(5.39737656850081E-17,1.79369009829332E-17,
-1.));
#14488=DIRECTION('ref_axis',(-1.,0.,-5.39737656850081E-17));
#14489=DIRECTION('',(-0.315367542755717,0.948969605928567,0.));
#14490=DIRECTION('',(0.948969605928567,0.315367542755717,5.68761795402233E-17));
#14491=DIRECTION('',(0.315367542755717,-0.948969605928567,3.08148791101958E-33));
#14492=DIRECTION('center_axis',(-0.671022843492016,-0.222998528048706,-0.707106781186547));
#14493=DIRECTION('ref_axis',(-0.725372545860843,-1.38777878078145E-17,0.688356498996966));
#14494=DIRECTION('',(0.671022843492016,0.222998528048706,-0.707106781186548));
#14495=DIRECTION('',(0.315367542755717,-0.948969605928568,-9.8130778667736E-18));
#14496=DIRECTION('center_axis',(0.67102284349202,0.22299852804872,0.70710678118654));
#14497=DIRECTION('ref_axis',(0.671022843491547,0.222998528050093,-0.707106781186555));
#14498=DIRECTION('center_axis',(-0.315367542755717,0.948969605928568,-2.77555756156289E-17));
#14499=DIRECTION('ref_axis',(-0.948969605928567,-0.315367542755717,0.));
#14500=DIRECTION('',(0.948969605928567,0.315367542755717,0.));
#14501=DIRECTION('center_axis',(-0.315367542755717,0.948969605928567,-2.77555756156289E-17));
#14502=DIRECTION('ref_axis',(-0.948969605928567,-0.315367542755718,-1.54074395550979E-33));
#14503=DIRECTION('center_axis',(-0.315367542755717,0.948969605928567,-2.77555756156289E-17));
#14504=DIRECTION('ref_axis',(-0.948969605928567,-0.315367542755718,-1.54074395550979E-33));
#14505=DIRECTION('center_axis',(0.,0.,1.));
#14506=DIRECTION('ref_axis',(-1.,0.,0.));
#14507=DIRECTION('center_axis',(0.,0.,1.));
#14508=DIRECTION('ref_axis',(-1.,0.,0.));
#14509=DIRECTION('center_axis',(0.,0.,1.));
#14510=DIRECTION('ref_axis',(-1.,0.,0.));
#14511=DIRECTION('center_axis',(0.,1.,0.));
#14512=DIRECTION('ref_axis',(0.,0.,1.));
#14513=DIRECTION('center_axis',(0.,1.,0.));
#14514=DIRECTION('ref_axis',(0.,0.,1.));
#14515=DIRECTION('center_axis',(0.,1.,0.));
#14516=DIRECTION('ref_axis',(0.,0.,1.));
#14517=DIRECTION('center_axis',(0.,1.,1.38777878078145E-16));
#14518=DIRECTION('ref_axis',(0.,-1.38777878078145E-16,1.));
#14519=DIRECTION('',(0.,-1.38777878078145E-16,1.));
#14520=DIRECTION('',(-1.,0.,0.));
#14521=DIRECTION('',(0.,-1.38777878078145E-16,1.));
#14522=DIRECTION('',(1.,0.,0.));
#14523=DIRECTION('center_axis',(0.,1.,3.85494105772624E-16));
#14524=DIRECTION('ref_axis',(0.,-3.85494105772624E-16,1.));
#14525=DIRECTION('center_axis',(0.,1.,3.85494105772624E-16));
#14526=DIRECTION('ref_axis',(0.,-3.85494105772624E-16,1.));
#14527=DIRECTION('center_axis',(0.,-1.,-1.23908819712629E-16));
#14528=DIRECTION('ref_axis',(0.,1.23908819712629E-16,-1.));
#14529=DIRECTION('',(0.,1.23908819712629E-16,-1.));
#14530=DIRECTION('',(-1.,0.,0.));
#14531=DIRECTION('',(0.,1.23908819712629E-16,-1.));
#14532=DIRECTION('',(1.,0.,0.));
#14533=DIRECTION('center_axis',(1.,0.,0.));
#14534=DIRECTION('ref_axis',(0.,0.,-1.));
#14535=DIRECTION('center_axis',(-1.,0.,0.));
#14536=DIRECTION('ref_axis',(0.,0.,-1.));
#14537=DIRECTION('',(0.,0.,-1.));
#14538=DIRECTION('center_axis',(1.,0.,0.));
#14539=DIRECTION('ref_axis',(0.,0.,-1.));
#14540=DIRECTION('center_axis',(1.,0.,0.));
#14541=DIRECTION('ref_axis',(0.,0.,-1.));
#14542=DIRECTION('',(0.,0.,-1.));
#14543=DIRECTION('center_axis',(-1.,0.,0.));
#14544=DIRECTION('ref_axis',(0.,1.06752213906265E-15,-1.));
#14545=DIRECTION('center_axis',(1.,0.,0.));
#14546=DIRECTION('ref_axis',(0.,0.,-1.));
#14547=DIRECTION('',(0.,0.,1.));
#14548=DIRECTION('center_axis',(1.,0.,0.));
#14549=DIRECTION('ref_axis',(0.,0.,-1.));
#14550=DIRECTION('center_axis',(1.,0.,0.));
#14551=DIRECTION('ref_axis',(0.,0.,-1.));
#14552=DIRECTION('',(0.,0.,1.));
#14553=DIRECTION('center_axis',(-1.,0.,0.));
#14554=DIRECTION('ref_axis',(0.,6.93889390390722E-15,-1.));
#14555=DIRECTION('center_axis',(-1.,0.,0.));
#14556=DIRECTION('ref_axis',(0.,-3.46944695195361E-15,-1.));
#14557=DIRECTION('center_axis',(0.315367542755717,-0.948969605928568,0.));
#14558=DIRECTION('ref_axis',(0.948969605928568,0.315367542755717,0.));
#14559=DIRECTION('center_axis',(0.315367542755717,-0.948969605928568,1.08947049901316E-33));
#14560=DIRECTION('ref_axis',(0.948969605928568,0.315367542755718,1.71056941445901E-49));
#14561=DIRECTION('center_axis',(0.315367542755717,-0.948969605928568,0.));
#14562=DIRECTION('ref_axis',(0.948969605928568,0.315367542755717,0.));
#14563=DIRECTION('center_axis',(0.315367542755717,-0.948969605928568,-2.17894099802631E-33));
#14564=DIRECTION('ref_axis',(0.948969605928568,0.315367542755718,-2.56585412168851E-49));
#14565=DIRECTION('center_axis',(0.,1.,0.));
#14566=DIRECTION('ref_axis',(0.,0.,1.));
#14567=DIRECTION('center_axis',(4.45059470661737E-15,-0.707106781186553,
0.707106781186542));
#14568=DIRECTION('ref_axis',(6.56775678445617E-13,-0.707106781186542,-0.707106781186553));
#14569=DIRECTION('center_axis',(0.,0.,1.));
#14570=DIRECTION('ref_axis',(1.,0.,0.));
#14571=DIRECTION('center_axis',(-0.129476575291326,0.,-0.991582480911613));
#14572=DIRECTION('ref_axis',(-0.991582480911613,0.,0.129476575291326));
#14573=DIRECTION('center_axis',(0.,1.,0.));
#14574=DIRECTION('ref_axis',(0.,0.,1.));
#14575=DIRECTION('center_axis',(0.,-1.,0.));
#14576=DIRECTION('ref_axis',(0.,0.,-1.));
#14577=DIRECTION('center_axis',(0.,1.,0.));
#14578=DIRECTION('ref_axis',(0.749352174952503,0.,-0.662171667993998));
#14579=DIRECTION('center_axis',(0.,-1.,0.));
#14580=DIRECTION('ref_axis',(0.,0.,-1.));
#14581=DIRECTION('center_axis',(-0.99997906305609,0.,0.00647096974680808));
#14582=DIRECTION('ref_axis',(0.00647096974680808,0.,0.99997906305609));
#14583=DIRECTION('center_axis',(0.99997906305609,0.,-0.00647096974680517));
#14584=DIRECTION('ref_axis',(-0.00647096974680517,0.,-0.99997906305609));
#14585=DIRECTION('center_axis',(-0.99997906305609,0.,0.00647096974681905));
#14586=DIRECTION('ref_axis',(0.00647096974681905,0.,0.99997906305609));
#14587=DIRECTION('center_axis',(1.,0.,0.));
#14588=DIRECTION('ref_axis',(0.,0.,1.));
#14589=DIRECTION('center_axis',(0.,0.,-1.));
#14590=DIRECTION('ref_axis',(1.,0.,0.));
#14591=DIRECTION('center_axis',(0.,1.,0.));
#14592=DIRECTION('ref_axis',(0.,0.,-1.));
#14593=DIRECTION('center_axis',(0.129476575291322,-1.7201214080047E-15,
-0.991582480911614));
#14594=DIRECTION('ref_axis',(0.991582480911614,6.93889390390724E-15,0.129476575291322));
#14595=DIRECTION('center_axis',(0.,0.,1.));
#14596=DIRECTION('ref_axis',(1.,0.,0.));
#14597=DIRECTION('center_axis',(0.,0.,-1.));
#14598=DIRECTION('ref_axis',(-1.,0.,0.));
#14599=DIRECTION('center_axis',(0.129476575291321,0.,-0.991582480911614));
#14600=DIRECTION('ref_axis',(-0.991582480911614,0.,-0.129476575291321));
#14601=DIRECTION('center_axis',(0.129476575291322,0.,-0.991582480911614));
#14602=DIRECTION('ref_axis',(-0.991582480911614,0.,-0.129476575291322));
#14603=DIRECTION('center_axis',(0.,-1.,0.));
#14604=DIRECTION('ref_axis',(-0.0648749531344188,0.,0.997893401348965));
#14605=DIRECTION('center_axis',(0.948969605928567,0.315367542755717,0.));
#14606=DIRECTION('ref_axis',(-0.315367542755717,0.948969605928568,0.));
#14607=DIRECTION('center_axis',(0.948969605928567,0.315367542755717,0.));
#14608=DIRECTION('ref_axis',(-0.315367542755717,0.948969605928568,0.));
#14609=DIRECTION('center_axis',(1.,0.,0.));
#14610=DIRECTION('ref_axis',(0.,0.,-1.));
#14611=DIRECTION('center_axis',(1.,0.,0.));
#14612=DIRECTION('ref_axis',(0.,0.,-1.));
#14613=DIRECTION('center_axis',(1.,0.,0.));
#14614=DIRECTION('ref_axis',(0.,0.,-1.));
#14615=DIRECTION('center_axis',(1.,0.,0.));
#14616=DIRECTION('ref_axis',(0.,0.,-1.));
#14617=DIRECTION('center_axis',(-0.948969605928567,-0.315367542755717,0.));
#14618=DIRECTION('ref_axis',(0.315367542755717,-0.948969605928567,0.));
#14619=DIRECTION('center_axis',(-0.948969605928567,-0.315367542755717,0.));
#14620=DIRECTION('ref_axis',(0.315367542755717,-0.948969605928567,0.));
#14621=DIRECTION('center_axis',(1.,0.,0.));
#14622=DIRECTION('ref_axis',(0.,0.,-1.));
#14623=DIRECTION('center_axis',(1.,0.,0.));
#14624=DIRECTION('ref_axis',(0.,0.,-1.));
#14625=DIRECTION('center_axis',(2.52323414687536E-15,0.,1.));
#14626=DIRECTION('ref_axis',(1.,0.,-2.52323414687536E-15));
#14627=DIRECTION('center_axis',(-0.129476575291322,0.,-0.991582480911614));
#14628=DIRECTION('ref_axis',(-0.991582480911614,0.,0.129476575291322));
#14629=DIRECTION('center_axis',(-2.52323414687536E-15,0.,1.));
#14630=DIRECTION('ref_axis',(1.,0.,2.52323414687536E-15));
#14631=DIRECTION('center_axis',(-2.31296463463574E-15,0.,1.));
#14632=DIRECTION('ref_axis',(1.,0.,2.31296463463574E-15));
#14633=DIRECTION('center_axis',(0.,-1.,0.));
#14634=DIRECTION('ref_axis',(-0.0648749531344198,0.,0.997893401348965));
#14635=DIRECTION('center_axis',(0.129476575291322,0.,-0.991582480911614));
#14636=DIRECTION('ref_axis',(-0.991582480911614,0.,-0.129476575291322));
#14637=DIRECTION('center_axis',(0.129476575291322,0.,-0.991582480911614));
#14638=DIRECTION('ref_axis',(-0.991582480911614,0.,-0.129476575291322));
#14639=DIRECTION('center_axis',(0.,0.,-1.));
#14640=DIRECTION('ref_axis',(-1.,0.,0.));
#14641=DIRECTION('center_axis',(0.,0.,1.));
#14642=DIRECTION('ref_axis',(1.,0.,0.));
#14643=DIRECTION('center_axis',(0.,0.,-1.));
#14644=DIRECTION('ref_axis',(-1.,0.,0.));
#14645=DIRECTION('center_axis',(0.,0.,1.));
#14646=DIRECTION('ref_axis',(1.,0.,0.));
#14647=DIRECTION('center_axis',(-1.26920068081332E-33,-4.21788745889624E-34,
-1.));
#14648=DIRECTION('ref_axis',(0.894021371540723,-0.448024315443308,-9.45720919282255E-34));
#14649=DIRECTION('center_axis',(0.,0.,1.));
#14650=DIRECTION('ref_axis',(1.,0.,0.));
#14651=DIRECTION('center_axis',(0.,0.,-1.));
#14652=DIRECTION('ref_axis',(-1.,0.,0.));
#14653=DIRECTION('center_axis',(1.,0.,0.));
#14654=DIRECTION('ref_axis',(0.,0.,-1.));
#14655=DIRECTION('center_axis',(1.,0.,0.));
#14656=DIRECTION('ref_axis',(0.,0.,-1.));
#14657=DIRECTION('axis',(0.,0.,1.));
#14658=DIRECTION('refdir',(1.,0.,0.));
#14659=DIRECTION('axis',(0.,0.,1.));
#14660=DIRECTION('refdir',(1.,0.,0.));
#14661=DIRECTION('center_axis',(0.,0.,1.));
#14662=DIRECTION('ref_axis',(0.723913745035715,0.689890491127661,0.));
#14663=DIRECTION('center_axis',(9.49460883474904E-17,-8.60566842858052E-17,
1.));
#14664=DIRECTION('ref_axis',(0.723913745035715,0.689890491127661,0.));
#14665=DIRECTION('',(0.,0.,1.));
#14666=DIRECTION('center_axis',(-9.47278923080924E-17,-4.21179355246917E-17,
-1.));
#14667=DIRECTION('ref_axis',(0.723913745035715,0.689890491127661,0.));
#14668=DIRECTION('',(0.,0.,-1.));
#14669=DIRECTION('center_axis',(9.49460883474904E-17,-8.60566842858052E-17,
1.));
#14670=DIRECTION('ref_axis',(0.999998551032278,0.00170233173745095,-9.47994537487936E-17));
#14671=DIRECTION('',(-0.689890491127661,0.723913745035715,1.27800020127394E-16));
#14672=DIRECTION('center_axis',(-9.49460883474904E-17,8.60566842858052E-17,
-1.));
#14673=DIRECTION('ref_axis',(0.444137634660357,0.89595857129574,0.));
#14674=DIRECTION('',(-0.993849755374348,0.110736912284699,1.03891798177174E-16));
#14675=DIRECTION('',(0.981518914375337,-0.191365150232375,-1.09659631875867E-16));
#14676=DIRECTION('center_axis',(9.49460883474904E-17,-8.60566842858052E-17,
1.));
#14677=DIRECTION('ref_axis',(0.999998551032278,0.00170233173745172,-9.47994537487935E-17));
#14678=DIRECTION('',(-0.984295785396816,-0.176527071153592,7.82637001701861E-17));
#14679=DIRECTION('',(0.00170233173745037,-0.999998551032278,-8.62181893319881E-17));
#14680=DIRECTION('center_axis',(-9.49460883474904E-17,8.60566842858052E-17,
-1.));
#14681=DIRECTION('ref_axis',(0.999998551032278,0.00170233173744927,-9.47994537487937E-17));
#14682=DIRECTION('',(0.999998551032278,0.00170233173745092,-9.47994537487935E-17));
#14683=DIRECTION('center_axis',(-9.49460883474904E-17,8.60566842858052E-17,
-1.));
#14684=DIRECTION('ref_axis',(0.999998551032278,0.00170233173744834,-9.47994537487938E-17));
#14685=DIRECTION('',(-0.175324395549563,0.984510719253569,1.01370093692115E-16));
#14686=DIRECTION('center_axis',(-9.49460883474904E-17,8.60566842858052E-17,
-1.));
#14687=DIRECTION('ref_axis',(0.999998551032278,0.00170233173745093,-9.47994537487936E-17));
#14688=DIRECTION('center_axis',(9.49460883474904E-17,-8.60566842858052E-17,
1.));
#14689=DIRECTION('ref_axis',(0.999998551032278,0.00170233173744927,-9.47994537487937E-17));
#14690=DIRECTION('center_axis',(9.49460883474904E-17,-8.60566842858052E-17,
1.));
#14691=DIRECTION('ref_axis',(0.999998551032278,0.00170233173745053,-9.47994537487936E-17));
#14692=DIRECTION('center_axis',(0.723913745035715,0.689890491127661,0.));
#14693=DIRECTION('ref_axis',(0.689890491127661,-0.723913745035715,0.));
#14694=DIRECTION('',(0.689890491127661,-0.723913745035715,-3.48621197090657E-17));
#14695=DIRECTION('',(0.,0.,1.));
#14696=DIRECTION('center_axis',(0.,0.,1.));
#14697=DIRECTION('ref_axis',(0.723913745035715,0.689890491127661,0.));
#14698=DIRECTION('center_axis',(9.47278923080924E-17,4.21179355246917E-17,
1.));
#14699=DIRECTION('ref_axis',(0.723913745035715,0.689890491127661,0.));
#14700=DIRECTION('',(0.,0.,1.));
#14701=DIRECTION('center_axis',(-9.49460883474904E-17,8.60566842858052E-17,
-1.));
#14702=DIRECTION('ref_axis',(0.723913745035715,0.689890491127661,0.));
#14703=DIRECTION('',(0.,0.,-1.));
#14704=DIRECTION('center_axis',(9.47278923080924E-17,4.21179355246917E-17,
1.));
#14705=DIRECTION('ref_axis',(0.00170233173745095,-0.999998551032278,4.19566161996647E-17));
#14706=DIRECTION('',(-0.689890491127661,0.723913745035715,3.48621197090657E-17));
#14707=DIRECTION('center_axis',(-9.47278923080924E-17,-4.21179355246917E-17,
-1.));
#14708=DIRECTION('ref_axis',(0.444137634660357,0.89595857129574,0.));
#14709=DIRECTION('',(-0.993849755374348,0.110736912284699,8.94812824657148E-17));
#14710=DIRECTION('',(0.981518914375337,-0.191365150232375,-8.49173129601425E-17));
#14711=DIRECTION('center_axis',(9.47278923080924E-17,4.21179355246917E-17,
1.));
#14712=DIRECTION('ref_axis',(0.00170233173745019,-0.999998551032278,4.19566161996648E-17));
#14713=DIRECTION('',(-0.984295785396816,-0.176527071153591,1.00675220959588E-16));
#14714=DIRECTION('',(0.00170233173745037,-0.999998551032278,4.19566161996648E-17));
#14715=DIRECTION('center_axis',(-9.47278923080924E-17,-4.21179355246917E-17,
-1.));
#14716=DIRECTION('ref_axis',(0.00170233173744927,-0.999998551032278,4.19566161996649E-17));
#14717=DIRECTION('',(-0.00170233173745037,0.999998551032278,8.62181893319882E-17));
#14718=DIRECTION('',(0.999998551032278,0.00170233173745037,-9.47994537487936E-17));
#14719=DIRECTION('',(-0.00170233173745037,0.999998551032278,8.62181893319881E-17));
#14720=DIRECTION('center_axis',(-9.47278923080924E-17,-4.21179355246917E-17,
-1.));
#14721=DIRECTION('ref_axis',(0.00170233173745089,-0.999998551032278,4.19566161996647E-17));
#14722=DIRECTION('',(-0.175324395549563,0.984510719253569,-2.48574485362892E-17));
#14723=DIRECTION('center_axis',(-9.47278923080924E-17,-4.21179355246917E-17,
-1.));
#14724=DIRECTION('ref_axis',(0.00170233173745093,-0.999998551032278,4.19566161996647E-17));
#14725=DIRECTION('center_axis',(9.47278923080924E-17,4.21179355246917E-17,
1.));
#14726=DIRECTION('ref_axis',(0.00170233173745116,-0.999998551032278,4.19566161996647E-17));
#14727=DIRECTION('center_axis',(9.47278923080924E-17,4.21179355246917E-17,
1.));
#14728=DIRECTION('ref_axis',(0.00170233173744927,-0.999998551032278,4.19566161996649E-17));
#14729=DIRECTION('center_axis',(9.47278923080924E-17,4.21179355246917E-17,
1.));
#14730=DIRECTION('ref_axis',(0.00170233173745101,-0.999998551032278,4.19566161996647E-17));
#14731=DIRECTION('center_axis',(0.723913745035715,0.689890491127661,0.));
#14732=DIRECTION('ref_axis',(0.689890491127661,-0.723913745035715,0.));
#14733=DIRECTION('',(0.689890491127661,-0.723913745035715,-1.27800020127394E-16));
#14734=DIRECTION('',(0.,0.,1.));
#14735=DIRECTION('center_axis',(0.,0.,-1.));
#14736=DIRECTION('ref_axis',(0.444137634660357,0.89595857129574,0.));
#14737=DIRECTION('center_axis',(9.47278923080924E-17,4.21179355246917E-17,
1.));
#14738=DIRECTION('ref_axis',(0.444137634660357,0.89595857129574,0.));
#14739=DIRECTION('',(0.,0.,-1.));
#14740=DIRECTION('center_axis',(0.110736912284699,0.993849755374348,0.));
#14741=DIRECTION('ref_axis',(0.993849755374348,-0.110736912284699,0.));
#14742=DIRECTION('',(0.993849755374348,-0.110736912284699,-8.94812824657148E-17));
#14743=DIRECTION('',(-8.08477301668617E-16,9.00823082713598E-17,1.));
#14744=DIRECTION('center_axis',(0.,0.,-1.));
#14745=DIRECTION('ref_axis',(0.444137634660357,0.89595857129574,0.));
#14746=DIRECTION('center_axis',(9.49460883474904E-17,-8.60566842858052E-17,
1.));
#14747=DIRECTION('ref_axis',(0.444137634660357,0.89595857129574,0.));
#14748=DIRECTION('',(0.,0.,-1.));
#14749=DIRECTION('center_axis',(0.110736912284699,0.993849755374348,0.));
#14750=DIRECTION('ref_axis',(0.993849755374348,-0.110736912284699,0.));
#14751=DIRECTION('',(0.993849755374348,-0.110736912284699,-1.03891798177174E-16));
#14752=DIRECTION('',(-8.08477301668617E-16,9.00823082713598E-17,1.));
#14753=DIRECTION('center_axis',(0.191365150232375,0.981518914375337,6.62968908743508E-17));
#14754=DIRECTION('ref_axis',(-0.981518914375337,0.191365150232375,1.09659631875867E-16));
#14755=DIRECTION('',(0.981518914375337,-0.191365150232375,-1.09659631875867E-16));
#14756=DIRECTION('',(-9.49460883474904E-17,8.60566842858052E-17,-1.));
#14757=DIRECTION('center_axis',(9.49460883474904E-17,-8.60566842858052E-17,
1.));
#14758=DIRECTION('ref_axis',(0.999998551032278,0.00170233173745095,-9.47994537487936E-17));
#14759=DIRECTION('center_axis',(9.49460883474904E-17,-8.60566842858052E-17,
1.));
#14760=DIRECTION('ref_axis',(0.999998551032278,0.00170233173745093,-9.47994537487936E-17));
#14761=DIRECTION('',(-0.175324395549563,0.984510719253569,1.01370093692115E-16));
#14762=DIRECTION('center_axis',(9.49460883474904E-17,-8.60566842858052E-17,
1.));
#14763=DIRECTION('ref_axis',(0.999998551032278,0.00170233173745112,-9.47994537487936E-17));
#14764=DIRECTION('',(-0.999998551032278,-0.00170233173745092,9.47994537487935E-17));
#14765=DIRECTION('center_axis',(9.49460883474904E-17,-8.60566842858052E-17,
1.));
#14766=DIRECTION('ref_axis',(0.999998551032278,0.00170233173744927,-9.47994537487937E-17));
#14767=DIRECTION('',(0.00170233173745037,-0.999998551032278,-8.62181893319881E-17));
#14768=DIRECTION('',(-0.984295785396816,-0.176527071153592,7.82637001701861E-17));
#14769=DIRECTION('center_axis',(-9.49460883474904E-17,8.60566842858052E-17,
-1.));
#14770=DIRECTION('ref_axis',(0.999998551032278,0.00170233173744519,-9.47994537487941E-17));
#14771=DIRECTION('center_axis',(9.49460883474904E-17,-8.60566842858052E-17,
1.));
#14772=DIRECTION('ref_axis',(0.999998551032278,0.00170233173745053,-9.47994537487936E-17));
#14773=DIRECTION('center_axis',(9.49460883474904E-17,-8.60566842858052E-17,
1.));
#14774=DIRECTION('ref_axis',(0.999998551032278,0.00170233173744927,-9.47994537487937E-17));
#14775=DIRECTION('center_axis',(0.191365150232375,0.981518914375337,6.62968908743508E-17));
#14776=DIRECTION('ref_axis',(-0.981518914375337,0.191365150232375,1.09659631875867E-16));
#14777=DIRECTION('',(-0.981518914375337,0.191365150232375,8.49173129601425E-17));
#14778=DIRECTION('',(-9.49460883474904E-17,8.60566842858052E-17,-1.));
#14779=DIRECTION('center_axis',(-9.49460883474904E-17,8.60566842858052E-17,
-1.));
#14780=DIRECTION('ref_axis',(-0.999998551032278,-0.00170233173745069,9.47994537487936E-17));
#14781=DIRECTION('center_axis',(-9.49460883474904E-17,8.60566842858052E-17,
-1.));
#14782=DIRECTION('ref_axis',(0.999998551032278,0.00170233173745204,-9.47994537487934E-17));
#14783=DIRECTION('',(-0.707105756611597,-0.00120373031538035,0.707106781186597));
#14784=DIRECTION('center_axis',(9.49460883474904E-17,-8.60566842858052E-17,
1.));
#14785=DIRECTION('ref_axis',(0.999998551032278,0.00170233173745069,-9.47994537487936E-17));
#14786=DIRECTION('center_axis',(9.49460883474904E-17,-8.60566842858052E-17,
1.));
#14787=DIRECTION('ref_axis',(0.999998551032278,0.00170233173745019,-9.47994537487936E-17));
#14788=DIRECTION('center_axis',(9.49460883474904E-17,-8.60566842858052E-17,
1.));
#14789=DIRECTION('ref_axis',(-0.999998551032278,-0.00170233173745204,9.47994537487934E-17));
#14790=DIRECTION('center_axis',(9.49460883474904E-17,-8.60566842858052E-17,
1.));
#14791=DIRECTION('ref_axis',(-0.999998551032278,-0.00170233173745204,9.47994537487934E-17));
#14792=DIRECTION('',(0.707105756611652,0.00120373031538027,-0.707106781186541));
#14793=DIRECTION('center_axis',(-9.49460883474904E-17,8.60566842858052E-17,
-1.));
#14794=DIRECTION('ref_axis',(-0.999998551032278,-0.00170233173745068,9.47994537487936E-17));
#14795=DIRECTION('center_axis',(9.49460883474904E-17,-8.60566842858052E-17,
1.));
#14796=DIRECTION('ref_axis',(0.999998551032278,0.00170233173745104,0.));
#14797=DIRECTION('center_axis',(9.49460883474904E-17,-8.60566842858052E-17,
1.));
#14798=DIRECTION('ref_axis',(0.999998551032278,0.00170233173745019,-9.47994537487936E-17));
#14799=DIRECTION('center_axis',(9.49460883474904E-17,-8.60566842858052E-17,
1.));
#14800=DIRECTION('ref_axis',(0.999998551032278,0.00170233173745019,-9.47994537487936E-17));
#14801=DIRECTION('center_axis',(9.49460883474904E-17,-8.60566842858052E-17,
1.));
#14802=DIRECTION('ref_axis',(0.999998551032278,0.00170233173745104,0.));
#14803=DIRECTION('center_axis',(-9.49460883474904E-17,8.60566842858052E-17,
-1.));
#14804=DIRECTION('ref_axis',(0.999998551032278,0.00170233173745019,-9.47994537487936E-17));
#14805=DIRECTION('center_axis',(-9.49460883474904E-17,8.60566842858052E-17,
-1.));
#14806=DIRECTION('ref_axis',(0.999998551032278,0.00170233173745019,-9.47994537487936E-17));
#14807=DIRECTION('center_axis',(-9.49460883474904E-17,8.60566842858052E-17,
-1.));
#14808=DIRECTION('ref_axis',(-0.999998551032278,-0.00170233173745053,9.47994537487936E-17));
#14809=DIRECTION('',(-9.49460883474904E-17,8.60566842858052E-17,-1.));
#14810=DIRECTION('center_axis',(-9.49460883474904E-17,8.60566842858052E-17,
-1.));
#14811=DIRECTION('ref_axis',(-0.999998551032278,-0.00170233173744927,9.47994537487937E-17));
#14812=DIRECTION('',(-9.49460883474904E-17,8.60566842858052E-17,-1.));
#14813=DIRECTION('center_axis',(-9.49460883474904E-17,8.60566842858052E-17,
-1.));
#14814=DIRECTION('ref_axis',(-0.999998551032278,-0.00170233173744927,9.47994537487937E-17));
#14815=DIRECTION('center_axis',(9.49460883474904E-17,-8.60566842858052E-17,
1.));
#14816=DIRECTION('ref_axis',(0.999998551032278,0.00170233173744927,-9.47994537487937E-17));
#14817=DIRECTION('',(-9.49460883474904E-17,8.60566842858052E-17,-1.));
#14818=DIRECTION('center_axis',(-9.49460883474904E-17,8.60566842858052E-17,
-1.));
#14819=DIRECTION('ref_axis',(-0.999998551032278,-0.00170233173745019,9.47994537487936E-17));
#14820=DIRECTION('',(9.49460883474904E-17,-8.60566842858052E-17,1.));
#14821=DIRECTION('center_axis',(-9.47278923080924E-17,-4.21179355246917E-17,
-1.));
#14822=DIRECTION('ref_axis',(-0.00170233173745019,0.999998551032278,-4.19566161996648E-17));
#14823=DIRECTION('',(-9.49460883474904E-17,8.60566842858052E-17,-1.));
#14824=DIRECTION('center_axis',(-9.49460883474904E-17,8.60566842858052E-17,
-1.));
#14825=DIRECTION('ref_axis',(-0.999998551032278,-0.00170233173745053,9.47994537487936E-17));
#14826=DIRECTION('center_axis',(-9.47278923080924E-17,-4.21179355246917E-17,
-1.));
#14827=DIRECTION('ref_axis',(-0.00170233173745115,0.999998551032278,-4.19566161996647E-17));
#14828=DIRECTION('',(-9.49460883474904E-17,8.60566842858052E-17,-1.));
#14829=DIRECTION('center_axis',(-9.49460883474904E-17,8.60566842858052E-17,
-1.));
#14830=DIRECTION('ref_axis',(-0.999998551032278,-0.00170233173744927,9.47994537487937E-17));
#14831=DIRECTION('center_axis',(-9.47278923080924E-17,-4.21179355246917E-17,
-1.));
#14832=DIRECTION('ref_axis',(-0.00170233173745101,0.999998551032278,-4.19566161996647E-17));
#14833=DIRECTION('',(-9.49460883474904E-17,8.60566842858052E-17,-1.));
#14834=DIRECTION('center_axis',(-9.49460883474904E-17,8.60566842858052E-17,
-1.));
#14835=DIRECTION('ref_axis',(-0.999998551032278,-0.00170233173744927,9.47994537487937E-17));
#14836=DIRECTION('center_axis',(-9.47278923080924E-17,-4.21179355246917E-17,
-1.));
#14837=DIRECTION('ref_axis',(-0.00170233173744927,0.999998551032278,-4.19566161996649E-17));
#14838=DIRECTION('',(-9.49460883474904E-17,8.60566842858052E-17,-1.));
#14839=DIRECTION('center_axis',(9.49460883474904E-17,-8.60566842858052E-17,
1.));
#14840=DIRECTION('ref_axis',(0.999998551032278,0.00170233173744927,-9.47994537487937E-17));
#14841=DIRECTION('center_axis',(-9.49460883474904E-17,8.60566842858052E-17,
-1.));
#14842=DIRECTION('ref_axis',(-0.999998551032278,-0.00170233173745019,9.47994537487936E-17));
#14843=DIRECTION('',(9.49460883474904E-17,-8.60566842858052E-17,1.));
#14844=DIRECTION('',(-9.49460883474904E-17,8.60566842858052E-17,-1.));
#14845=DIRECTION('center_axis',(-0.00170233173745037,0.999998551032278,
8.62181893319881E-17));
#14846=DIRECTION('ref_axis',(-0.999998551032278,-0.00170233173745037,9.47994537487936E-17));
#14847=DIRECTION('',(3.42763368692988E-16,-8.56348164531116E-17,1.));
#14848=DIRECTION('',(0.999998551032278,0.00170233173745037,-9.47994537487936E-17));
#14849=DIRECTION('',(-9.49460883474904E-17,8.60566842858052E-17,-1.));
#14850=DIRECTION('',(-0.999998551032278,-0.00170233173745037,9.47994537487936E-17));
#14851=DIRECTION('center_axis',(-9.49460883474904E-17,8.60566842858052E-17,
-1.));
#14852=DIRECTION('ref_axis',(-0.999998551032278,-0.00170233173745112,9.47994537487936E-17));
#14853=DIRECTION('',(-9.49460883474904E-17,8.60566842858052E-17,-1.));
#14854=DIRECTION('',(9.49460883474904E-17,-8.60566842858052E-17,1.));
#14855=DIRECTION('',(-9.49460883474904E-17,8.60566842858052E-17,-1.));
#14856=DIRECTION('center_axis',(9.47278923080924E-17,4.21179355246917E-17,
1.));
#14857=DIRECTION('ref_axis',(-0.00170233173744927,0.999998551032278,-4.19566161996649E-17));
#14858=DIRECTION('',(9.49460883474904E-17,-8.60566842858052E-17,1.));
#14859=DIRECTION('center_axis',(-9.49460883474904E-17,8.60566842858052E-17,
-1.));
#14860=DIRECTION('ref_axis',(-0.999998551032278,-0.00170233173744927,9.47994537487937E-17));
#14861=DIRECTION('',(9.49460883474904E-17,-8.60566842858052E-17,1.));
#14862=DIRECTION('',(-9.49460883474904E-17,8.60566842858052E-17,-1.));
#14863=DIRECTION('center_axis',(9.47278923080924E-17,4.21179355246917E-17,
1.));
#14864=DIRECTION('ref_axis',(-0.00170233173745274,0.999998551032278,-4.19566161996646E-17));
#14865=DIRECTION('',(9.49460883474904E-17,-8.60566842858052E-17,1.));
#14866=DIRECTION('',(-9.49460883474904E-17,8.60566842858052E-17,-1.));
#14867=DIRECTION('center_axis',(0.999998551032278,0.00170233173745037,-9.47994537487936E-17));
#14868=DIRECTION('ref_axis',(-0.00170233173745037,0.999998551032278,8.62181893319882E-17));
#14869=DIRECTION('',(-9.49460883474904E-17,8.60566842858052E-17,-1.));
#14870=DIRECTION('center_axis',(-0.984510719253569,-0.175324395549563,7.83876055738923E-17));
#14871=DIRECTION('ref_axis',(0.175324395549563,-0.984510719253569,-1.01370093692115E-16));
#14872=DIRECTION('',(0.175324395549563,-0.984510719253569,2.48574485362892E-17));
#14873=DIRECTION('',(-9.49460883474904E-17,8.60566842858052E-17,-1.));
#14874=DIRECTION('center_axis',(0.176527071153592,-0.984295785396816,-1.01465786541215E-16));
#14875=DIRECTION('ref_axis',(0.984295785396816,0.176527071153592,-7.8263700170186E-17));
#14876=DIRECTION('',(0.984295785396816,0.176527071153591,-1.00675220959588E-16));
#14877=DIRECTION('',(-9.49460883474904E-17,8.60566842858052E-17,-1.));
#14878=DIRECTION('center_axis',(-0.984510719253569,-0.175324395549563,7.83876055738923E-17));
#14879=DIRECTION('ref_axis',(0.175324395549563,-0.984510719253569,-1.01370093692115E-16));
#14880=DIRECTION('',(-9.49460883474904E-17,8.60566842858052E-17,-1.));
#14881=DIRECTION('center_axis',(0.00170233173745092,-0.999998551032278,
-8.62181893319882E-17));
#14882=DIRECTION('ref_axis',(0.999998551032278,0.00170233173745092,-9.47994537487936E-17));
#14883=DIRECTION('',(-0.999998551032278,-0.00170233173745092,9.47994537487935E-17));
#14884=DIRECTION('',(0.999998551032278,0.00170233173745092,-9.47994537487935E-17));
#14885=DIRECTION('center_axis',(0.999998551032278,0.00170233173745037,-9.47994537487936E-17));
#14886=DIRECTION('ref_axis',(-0.00170233173745037,0.999998551032278,8.62181893319882E-17));
#14887=DIRECTION('',(-0.00170233173745037,0.999998551032278,-4.19566161996648E-17));
#14888=DIRECTION('center_axis',(0.176527071153592,-0.984295785396816,-1.01465786541215E-16));
#14889=DIRECTION('ref_axis',(0.984295785396816,0.176527071153592,-7.8263700170186E-17));
#14890=DIRECTION('center_axis',(-9.47278923080924E-17,-4.21179355246917E-17,
-1.));
#14891=DIRECTION('ref_axis',(-0.00170233173745095,0.999998551032278,-4.19566161996647E-17));
#14892=DIRECTION('center_axis',(9.47278923080924E-17,4.21179355246917E-17,
1.));
#14893=DIRECTION('ref_axis',(-0.00170233173745177,0.999998551032278,-4.19566161996647E-17));
#14894=DIRECTION('',(-0.00170233173745037,0.999998551032278,8.62181893319881E-17));
#14895=DIRECTION('',(-0.999998551032278,-0.00170233173745037,9.47994537487936E-17));
#14896=DIRECTION('',(-0.00170233173745037,0.999998551032278,8.62181893319882E-17));
#14897=DIRECTION('center_axis',(9.49460883474904E-17,-8.60566842858052E-17,
1.));
#14898=DIRECTION('ref_axis',(0.999998551032278,0.00170233173745095,-9.47994537487936E-17));
#14899=DIRECTION('center_axis',(-9.49460883474904E-17,8.60566842858052E-17,
-1.));
#14900=DIRECTION('ref_axis',(0.999998551032278,0.00170233173745095,-9.47994537487936E-17));
#14901=DIRECTION('center_axis',(-9.49460883474904E-17,8.60566842858052E-17,
-1.));
#14902=DIRECTION('ref_axis',(0.807462267669275,-0.589919220139836,-1.27431875885094E-16));
#14903=DIRECTION('center_axis',(-9.49460883474904E-17,8.60566842858052E-17,
-1.));
#14904=DIRECTION('ref_axis',(0.807462267669275,-0.589919220139835,-1.27431875885094E-16));
#14905=DIRECTION('center_axis',(-0.999998551032278,-0.00170233173745037,
3.42617093174052E-16));
#14906=DIRECTION('ref_axis',(0.00170233173745037,-0.999998551032278,-8.62181893319881E-17));
#14907=DIRECTION('center_axis',(0.999998551032278,0.00170233173745037,-3.42617093174052E-16));
#14908=DIRECTION('ref_axis',(0.00170233173745037,-0.999998551032278,-3.76615600624924E-31));
#14909=DIRECTION('center_axis',(0.999998551032278,0.00170233173745037,-3.42617093174052E-16));
#14910=DIRECTION('ref_axis',(0.00170233173745037,-0.999998551032278,-3.76615600624924E-31));
#14911=DIRECTION('center_axis',(0.999998551032278,0.00170233173745037,-9.47994537487936E-17));
#14912=DIRECTION('ref_axis',(-0.00170233173745037,0.999998551032278,8.62181893319882E-17));
#14913=DIRECTION('center_axis',(-0.999998551032278,-0.00170233173745037,
9.47994537487936E-17));
#14914=DIRECTION('ref_axis',(-0.00170233173745037,0.999998551032278,1.04216884115654E-31));
#14915=DIRECTION('center_axis',(-0.999998551032278,-0.00170233173745037,
9.47994537487936E-17));
#14916=DIRECTION('ref_axis',(-0.00170233173745037,0.999998551032278,1.04216884115654E-31));
#14917=DIRECTION('center_axis',(-0.999998551032278,-0.00170233173745092,
9.47994537487936E-17));
#14918=DIRECTION('ref_axis',(0.00170233173745092,-0.999998551032278,1.06889111913492E-31));
#14919=DIRECTION('center_axis',(0.999998551032278,0.00170233173745092,-9.47994537487936E-17));
#14920=DIRECTION('ref_axis',(-0.00170233173745092,0.999998551032278,-1.06889111913492E-31));
#14921=DIRECTION('center_axis',(0.999998551032278,0.00170233173745037,-9.47994537487936E-17));
#14922=DIRECTION('ref_axis',(-0.00170233173745037,0.999998551032278,1.04216884115654E-31));
#14923=DIRECTION('center_axis',(0.999998551032278,0.00170233173745037,-9.47994537487936E-17));
#14924=DIRECTION('ref_axis',(-0.00170233173745037,0.999998551032278,1.04216884115654E-31));
#14925=DIRECTION('axis',(0.,0.,1.));
#14926=DIRECTION('refdir',(1.,0.,0.));
#14927=DIRECTION('center_axis',(0.,0.,1.));
#14928=DIRECTION('ref_axis',(1.,0.,0.));
#14929=DIRECTION('center_axis',(0.,0.,1.));
#14930=DIRECTION('ref_axis',(-1.,0.,0.));
#14931=DIRECTION('',(0.707106781186555,8.65956056235502E-17,-0.70710678118654));
#14932=DIRECTION('center_axis',(0.,0.,-1.));
#14933=DIRECTION('ref_axis',(-1.,0.,0.));
#14934=DIRECTION('center_axis',(0.,0.,-1.));
#14935=DIRECTION('ref_axis',(-1.,0.,0.));
#14936=DIRECTION('center_axis',(0.,0.,-1.));
#14937=DIRECTION('ref_axis',(1.,0.,0.));
#14938=DIRECTION('',(-0.70710678118654,8.65956056235484E-17,0.707106781186555));
#14939=DIRECTION('center_axis',(0.,0.,1.));
#14940=DIRECTION('ref_axis',(1.,0.,0.));
#14941=DIRECTION('center_axis',(0.,0.,1.));
#14942=DIRECTION('ref_axis',(1.,0.,0.));
#14943=DIRECTION('center_axis',(0.,0.,1.));
#14944=DIRECTION('ref_axis',(1.,0.,0.));
#14945=DIRECTION('center_axis',(0.,0.,1.));
#14946=DIRECTION('ref_axis',(1.,0.,0.));
#14947=DIRECTION('',(0.707106781186552,8.65956056235499E-17,-0.707106781186543));
#14948=DIRECTION('center_axis',(0.,0.,-1.));
#14949=DIRECTION('ref_axis',(1.,0.,0.));
#14950=DIRECTION('center_axis',(0.,0.,1.));
#14951=DIRECTION('ref_axis',(1.,0.,0.));
#14952=DIRECTION('center_axis',(0.,0.,-1.));
#14953=DIRECTION('ref_axis',(-1.,0.,0.));
#14954=DIRECTION('',(0.,0.,-1.));
#14955=DIRECTION('center_axis',(0.,0.,-1.));
#14956=DIRECTION('ref_axis',(-1.,0.,0.));
#14957=DIRECTION('',(0.,0.,1.));
#14958=DIRECTION('center_axis',(0.,0.,1.));
#14959=DIRECTION('ref_axis',(1.,0.,0.));
#14960=DIRECTION('center_axis',(0.,0.,1.));
#14961=DIRECTION('ref_axis',(1.,0.,0.));
#14962=DIRECTION('center_axis',(0.,0.,-1.));
#14963=DIRECTION('ref_axis',(1.,0.,0.));
#14964=DIRECTION('center_axis',(0.,0.,-1.));
#14965=DIRECTION('ref_axis',(1.,0.,0.));
#14966=DIRECTION('center_axis',(0.,0.,1.));
#14967=DIRECTION('ref_axis',(-1.,0.,0.));
#14968=DIRECTION('',(0.707106781186555,-8.65956056235502E-17,0.70710678118654));
#14969=DIRECTION('center_axis',(0.,0.,-1.));
#14970=DIRECTION('ref_axis',(-1.,0.,0.));
#14971=DIRECTION('center_axis',(0.,0.,1.));
#14972=DIRECTION('ref_axis',(-1.,0.,0.));
#14973=DIRECTION('center_axis',(0.,0.,-1.));
#14974=DIRECTION('ref_axis',(1.,0.,0.));
#14975=DIRECTION('',(-0.70710678118654,-8.65956056235484E-17,-0.707106781186555));
#14976=DIRECTION('center_axis',(0.,0.,1.));
#14977=DIRECTION('ref_axis',(1.,0.,0.));
#14978=DIRECTION('center_axis',(0.,0.,-1.));
#14979=DIRECTION('ref_axis',(1.,0.,0.));
#14980=DIRECTION('center_axis',(0.,0.,1.));
#14981=DIRECTION('ref_axis',(1.,0.,0.));
#14982=DIRECTION('',(0.707106781186552,-8.65956056235499E-17,0.707106781186543));
#14983=DIRECTION('center_axis',(0.,0.,-1.));
#14984=DIRECTION('ref_axis',(1.,0.,0.));
#14985=DIRECTION('center_axis',(0.,0.,1.));
#14986=DIRECTION('ref_axis',(1.,0.,0.));
#14987=DIRECTION('center_axis',(0.,0.,-1.));
#14988=DIRECTION('ref_axis',(1.,0.,0.));
#14989=DIRECTION('center_axis',(0.,0.,-1.));
#14990=DIRECTION('ref_axis',(-1.,0.,0.));
#14991=DIRECTION('',(0.,0.,1.));
#14992=DIRECTION('center_axis',(0.,0.,1.));
#14993=DIRECTION('ref_axis',(-1.,0.,0.));
#14994=DIRECTION('',(0.,0.,-1.));
#14995=DIRECTION('center_axis',(0.,0.,-1.));
#14996=DIRECTION('ref_axis',(1.,0.,0.));
#14997=DIRECTION('center_axis',(0.,0.,-1.));
#14998=DIRECTION('ref_axis',(1.,0.,0.));
#14999=DIRECTION('center_axis',(0.,0.,1.));
#15000=DIRECTION('ref_axis',(1.,0.,0.));
#15001=DIRECTION('',(0.,0.,1.));
#15002=DIRECTION('',(1.,0.,0.));
#15003=DIRECTION('',(0.,0.,1.));
#15004=DIRECTION('',(1.,0.,0.));
#15005=DIRECTION('axis',(0.,0.,1.));
#15006=DIRECTION('refdir',(1.,0.,0.));
#15007=DIRECTION('axis',(0.,0.,1.));
#15008=DIRECTION('refdir',(1.,0.,0.));
#15009=DIRECTION('center_axis',(-0.0498412966806708,0.998757150234825,2.18495763504859E-17));
#15010=DIRECTION('ref_axis',(0.695179757024366,0.0346917771833739,0.717998318953048));
#15011=DIRECTION('center_axis',(-0.0498412966806708,0.998757150234825,2.18495763504859E-17));
#15012=DIRECTION('ref_axis',(0.695179757024367,0.034691777183374,0.717998318953046));
#15013=DIRECTION('center_axis',(-0.0498412966806708,0.998757150234825,2.18495763504859E-17));
#15014=DIRECTION('ref_axis',(0.695179757024367,0.034691777183374,0.717998318953046));
#15015=DIRECTION('',(0.526809439201579,-0.68169716279182,0.507701480212241));
#15016=DIRECTION('center_axis',(0.0498412966806708,-0.998757150234825,-2.18495763504859E-17));
#15017=DIRECTION('ref_axis',(0.69517975702437,0.0346917771833741,0.717998318953044));
#15018=DIRECTION('center_axis',(0.0498412966806708,-0.998757150234825,-2.18495763504859E-17));
#15019=DIRECTION('ref_axis',(-0.695179757024368,-0.034691777183374,-0.717998318953046));
#15020=DIRECTION('center_axis',(-0.0498412966806708,0.998757150234825,2.18495763504859E-17));
#15021=DIRECTION('ref_axis',(-0.695179757024368,-0.034691777183374,-0.717998318953046));
#15022=DIRECTION('center_axis',(0.0498412966806708,-0.998757150234825,-2.18495763504859E-17));
#15023=DIRECTION('ref_axis',(0.69517975702437,0.0346917771833741,0.717998318953044));
#15024=DIRECTION('center_axis',(0.695179757024367,0.0346917771833744,0.717998318953047));
#15025=DIRECTION('ref_axis',(0.71710595491094,0.0357859672311607,-0.696044836185572));
#15026=DIRECTION('center_axis',(-0.0498412966806708,0.998757150234825,2.18495763504859E-17));
#15027=DIRECTION('ref_axis',(-0.695179757024368,-0.034691777183374,-0.717998318953046));
#15028=DIRECTION('center_axis',(-0.526809439201581,0.681697162791818,-0.507701480212242));
#15029=DIRECTION('ref_axis',(-0.456323201469511,-0.730758744587374,-0.507701480212241));
#15030=DIRECTION('center_axis',(-0.0498412966806708,0.998757150234825,2.18495763504859E-17));
#15031=DIRECTION('ref_axis',(-0.695179757024366,-0.0346917771833739,-0.717998318953048));
#15032=DIRECTION('center_axis',(0.47182736468075,0.731532453790069,-0.492178023676697));
#15033=DIRECTION('ref_axis',(0.542313602412785,-0.680923453589126,-0.492178023676724));
#15034=DIRECTION('center_axis',(-0.0498412966806708,0.998757150234825,2.18495763504859E-17));
#15035=DIRECTION('ref_axis',(-0.695179757024368,-0.034691777183374,-0.717998318953046));
#15036=DIRECTION('center_axis',(-0.542313602412816,0.680923453589121,0.492178023676697));
#15037=DIRECTION('ref_axis',(0.471827364680741,0.731532453790072,-0.492178023676701));
#15038=DIRECTION('center_axis',(-0.0498412966806708,0.998757150234825,2.18495763504859E-17));
#15039=DIRECTION('ref_axis',(-0.695179757024374,-0.0346917771833743,-0.71799831895304));
#15040=DIRECTION('center_axis',(-0.526809439201581,0.681697162791818,-0.507701480212242));
#15041=DIRECTION('ref_axis',(-0.456323201469524,-0.730758744587375,-0.507701480212228));
#15042=DIRECTION('center_axis',(-0.0498412966806708,0.998757150234825,2.18495763504859E-17));
#15043=DIRECTION('ref_axis',(-0.695179757024368,-0.034691777183374,-0.717998318953046));
#15044=DIRECTION('center_axis',(0.456323201469515,0.730758744587371,0.507701480212242));
#15045=DIRECTION('ref_axis',(-0.526809439201585,0.681697162791821,-0.507701480212233));
#15046=DIRECTION('center_axis',(-0.0498412966806708,0.998757150234825,2.18495763504859E-17));
#15047=DIRECTION('ref_axis',(-0.695179757024363,-0.0346917771833738,-0.71799831895305));
#15048=DIRECTION('center_axis',(-0.542313602412816,0.680923453589121,0.492178023676697));
#15049=DIRECTION('ref_axis',(0.471827364680746,0.731532453790072,-0.492178023676696));
#15050=DIRECTION('center_axis',(-0.0498412966806708,0.998757150234825,2.18495763504859E-17));
#15051=DIRECTION('ref_axis',(-0.69517975702437,-0.0346917771833741,-0.717998318953044));
#15052=DIRECTION('center_axis',(0.47182736468075,0.731532453790069,-0.492178023676697));
#15053=DIRECTION('ref_axis',(0.542313602412809,-0.680923453589124,-0.492178023676699));
#15054=DIRECTION('center_axis',(-0.0498412966806708,0.998757150234825,2.18495763504859E-17));
#15055=DIRECTION('ref_axis',(-0.695179757024366,-0.0346917771833739,-0.717998318953048));
#15056=DIRECTION('center_axis',(0.456323201469515,0.730758744587371,0.507701480212242));
#15057=DIRECTION('ref_axis',(-0.526809439201583,0.681697162791821,-0.507701480212235));
#15058=DIRECTION('center_axis',(-0.695179757024368,-0.0346917771833739,
-0.717998318953046));
#15059=DIRECTION('ref_axis',(-0.71710595491094,-0.0357859672311622,0.696044836185572));
#15060=DIRECTION('center_axis',(0.0498412966806708,-0.998757150234825,-2.18495763504859E-17));
#15061=DIRECTION('ref_axis',(0.695179757024368,0.034691777183374,0.717998318953046));
#15062=DIRECTION('center_axis',(-0.456323201469515,-0.730758744587371,-0.507701480212242));
#15063=DIRECTION('ref_axis',(-0.526809439201578,0.681697162791822,-0.50770148021224));
#15064=DIRECTION('center_axis',(0.0498412966806708,-0.998757150234825,-2.18495763504859E-17));
#15065=DIRECTION('ref_axis',(-0.695179757024368,-0.034691777183374,-0.717998318953046));
#15066=DIRECTION('center_axis',(-0.47182736468075,-0.731532453790069,0.492178023676697));
#15067=DIRECTION('ref_axis',(0.542313602412811,-0.680923453589124,-0.492178023676697));
#15068=DIRECTION('center_axis',(0.542313602412816,-0.680923453589121,-0.492178023676697));
#15069=DIRECTION('ref_axis',(0.471827364680746,0.731532453790072,-0.492178023676696));
#15070=DIRECTION('center_axis',(0.0498412966806708,-0.998757150234825,-2.18495763504859E-17));
#15071=DIRECTION('ref_axis',(-0.695179757024368,-0.034691777183374,-0.717998318953046));
#15072=DIRECTION('center_axis',(-0.456323201469515,-0.730758744587371,-0.507701480212242));
#15073=DIRECTION('ref_axis',(-0.526809439201578,0.681697162791822,-0.50770148021224));
#15074=DIRECTION('center_axis',(0.0498412966806708,-0.998757150234825,-2.18495763504859E-17));
#15075=DIRECTION('ref_axis',(0.695179757024362,0.0346917771833737,0.717998318953052));
#15076=DIRECTION('center_axis',(0.526809439201581,-0.681697162791818,0.507701480212242));
#15077=DIRECTION('ref_axis',(-0.456323201469513,-0.730758744587375,-0.507701480212239));
#15078=DIRECTION('center_axis',(0.0498412966806708,-0.998757150234825,-2.18495763504859E-17));
#15079=DIRECTION('ref_axis',(-0.695179757024368,-0.034691777183374,-0.717998318953046));
#15080=DIRECTION('center_axis',(0.542313602412816,-0.680923453589121,-0.492178023676697));
#15081=DIRECTION('ref_axis',(0.471827364680746,0.731532453790072,-0.492178023676696));
#15082=DIRECTION('center_axis',(0.0498412966806708,-0.998757150234825,-2.18495763504859E-17));
#15083=DIRECTION('ref_axis',(0.695179757024367,0.034691777183374,0.717998318953047));
#15084=DIRECTION('center_axis',(-0.47182736468075,-0.731532453790069,0.492178023676697));
#15085=DIRECTION('ref_axis',(0.542313602412811,-0.680923453589124,-0.492178023676697));
#15086=DIRECTION('center_axis',(0.0498412966806708,-0.998757150234825,-2.18495763504859E-17));
#15087=DIRECTION('ref_axis',(-0.695179757024368,-0.034691777183374,-0.717998318953046));
#15088=DIRECTION('center_axis',(0.526809439201581,-0.681697162791818,0.507701480212242));
#15089=DIRECTION('ref_axis',(-0.456323201469513,-0.730758744587375,-0.507701480212239));
#15090=DIRECTION('center_axis',(0.0498412966806708,-0.998757150234825,-2.18495763504859E-17));
#15091=DIRECTION('ref_axis',(-0.695179757024367,-0.034691777183374,-0.717998318953046));
#15092=DIRECTION('center_axis',(0.0498412966806708,-0.998757150234825,-2.18495763504859E-17));
#15093=DIRECTION('ref_axis',(-0.695179757024367,-0.034691777183374,-0.717998318953046));
#15094=DIRECTION('',(-0.0498412966806708,0.998757150234825,2.18495763504859E-17));
#15095=DIRECTION('center_axis',(0.0498412966806708,-0.998757150234825,-2.18495763504859E-17));
#15096=DIRECTION('ref_axis',(-0.695179757024367,-0.034691777183374,-0.717998318953047));
#15097=DIRECTION('center_axis',(0.0498412966806708,-0.998757150234825,-2.18495763504859E-17));
#15098=DIRECTION('ref_axis',(-0.695179757024368,-0.034691777183374,-0.717998318953046));
#15099=DIRECTION('center_axis',(0.0498412966806708,-0.998757150234825,-2.18495763504859E-17));
#15100=DIRECTION('ref_axis',(-0.695179757024367,-0.034691777183374,-0.717998318953047));
#15101=DIRECTION('center_axis',(0.0498412966806708,-0.998757150234825,-2.18495763504859E-17));
#15102=DIRECTION('ref_axis',(-0.695179757024368,-0.034691777183374,-0.717998318953046));
#15103=DIRECTION('center_axis',(0.0498412966806708,-0.998757150234825,-2.18495763504859E-17));
#15104=DIRECTION('ref_axis',(-0.695179757024367,-0.034691777183374,-0.717998318953047));
#15105=DIRECTION('center_axis',(0.0498412966806708,-0.998757150234825,-2.18495763504859E-17));
#15106=DIRECTION('ref_axis',(-0.695179757024368,-0.034691777183374,-0.717998318953046));
#15107=DIRECTION('center_axis',(-0.0498412966806708,0.998757150234825,1.38777878078145E-17));
#15108=DIRECTION('ref_axis',(0.695179757024368,0.034691777183374,0.717998318953046));
#15109=DIRECTION('center_axis',(0.0498412966806708,-0.998757150234825,-2.18495763504859E-17));
#15110=DIRECTION('ref_axis',(-0.695179757024367,-0.034691777183374,-0.717998318953047));
#15111=DIRECTION('center_axis',(0.0498412966806708,-0.998757150234825,-2.18495763504859E-17));
#15112=DIRECTION('ref_axis',(-0.695179757024368,-0.034691777183374,-0.717998318953046));
#15113=DIRECTION('center_axis',(0.0498412966806708,-0.998757150234825,-1.38777878078145E-17));
#15114=DIRECTION('ref_axis',(-0.695179757024368,-0.034691777183374,-0.717998318953046));
#15115=DIRECTION('',(0.71710595491094,0.0357859672311617,-0.696044836185572));
#15116=DIRECTION('center_axis',(-0.0498412966806708,0.998757150234825,2.18495763504859E-17));
#15117=DIRECTION('ref_axis',(-0.695179757024367,-0.034691777183374,-0.717998318953047));
#15118=DIRECTION('',(0.71710595491094,0.0357859672311617,-0.696044836185572));
#15119=DIRECTION('center_axis',(-0.456323201469515,-0.730758744587371,-0.507701480212242));
#15120=DIRECTION('ref_axis',(-0.526809439201578,0.681697162791822,-0.507701480212239));
#15121=DIRECTION('',(-0.71710595491094,-0.0357859672311617,0.696044836185572));
#15122=DIRECTION('center_axis',(0.526809439201581,-0.681697162791818,0.507701480212242));
#15123=DIRECTION('ref_axis',(-0.456323201469513,-0.730758744587375,-0.507701480212239));
#15124=DIRECTION('',(0.71710595491094,0.0357859672311617,-0.696044836185572));
#15125=DIRECTION('center_axis',(0.526809439201581,-0.681697162791818,0.507701480212242));
#15126=DIRECTION('ref_axis',(-0.456323201469513,-0.730758744587375,-0.507701480212239));
#15127=DIRECTION('',(0.71710595491094,0.0357859672311617,-0.696044836185572));
#15128=DIRECTION('',(0.71710595491094,0.0357859672311617,-0.696044836185572));
#15129=DIRECTION('center_axis',(-0.456323201469515,-0.730758744587371,-0.507701480212242));
#15130=DIRECTION('ref_axis',(-0.526809439201578,0.681697162791822,-0.507701480212239));
#15131=DIRECTION('',(-0.71710595491094,-0.0357859672311617,0.696044836185572));
#15132=DIRECTION('',(0.71710595491094,0.0357859672311617,-0.696044836185572));
#15133=DIRECTION('center_axis',(0.0498412966806708,-0.998757150234825,-1.38777878078145E-17));
#15134=DIRECTION('ref_axis',(-0.695179757024368,-0.034691777183374,-0.717998318953046));
#15135=DIRECTION('center_axis',(-0.0498412966806708,0.998757150234825,2.18495763504859E-17));
#15136=DIRECTION('ref_axis',(-0.695179757024368,-0.034691777183374,-0.717998318953046));
#15137=DIRECTION('center_axis',(0.0498412966806708,-0.998757150234825,-1.38777878078145E-17));
#15138=DIRECTION('ref_axis',(-0.695179757024368,-0.034691777183374,-0.717998318953046));
#15139=DIRECTION('',(0.695179757024365,0.0346917771833739,0.717998318953049));
#15140=DIRECTION('',(0.695179757024365,0.0346917771833739,0.717998318953049));
#15141=DIRECTION('center_axis',(0.542313602412816,-0.68092345358912,-0.492178023676697));
#15142=DIRECTION('ref_axis',(0.471827364680746,0.731532453790072,-0.492178023676696));
#15143=DIRECTION('',(-0.695179757024365,-0.0346917771833739,-0.717998318953049));
#15144=DIRECTION('center_axis',(-0.47182736468075,-0.731532453790069,0.492178023676697));
#15145=DIRECTION('ref_axis',(0.542313602412812,-0.680923453589124,-0.492178023676696));
#15146=DIRECTION('',(0.695179757024365,0.0346917771833739,0.717998318953049));
#15147=DIRECTION('center_axis',(-0.47182736468075,-0.731532453790069,0.492178023676697));
#15148=DIRECTION('ref_axis',(0.542313602412812,-0.680923453589124,-0.492178023676696));
#15149=DIRECTION('',(0.695179757024365,0.0346917771833739,0.717998318953049));
#15150=DIRECTION('',(0.695179757024365,0.0346917771833739,0.717998318953049));
#15151=DIRECTION('center_axis',(0.542313602412816,-0.68092345358912,-0.492178023676697));
#15152=DIRECTION('ref_axis',(0.471827364680746,0.731532453790072,-0.492178023676696));
#15153=DIRECTION('',(-0.695179757024365,-0.0346917771833739,-0.717998318953049));
#15154=DIRECTION('',(0.695179757024365,0.0346917771833739,0.717998318953049));
#15155=DIRECTION('center_axis',(0.0498412966806708,-0.998757150234825,-1.38777878078145E-17));
#15156=DIRECTION('ref_axis',(-0.695179757024368,-0.034691777183374,-0.717998318953046));
#15157=DIRECTION('center_axis',(-0.0498412966806708,0.998757150234825,2.18495763504859E-17));
#15158=DIRECTION('ref_axis',(-0.695179757024368,-0.034691777183374,-0.717998318953046));
#15159=DIRECTION('center_axis',(0.0498412966806708,-0.998757150234825,-1.04083408558608E-17));
#15160=DIRECTION('ref_axis',(-0.695179757024368,-0.034691777183374,-0.717998318953046));
#15161=DIRECTION('center_axis',(0.0498412966806708,-0.998757150234825,-1.04083408558608E-17));
#15162=DIRECTION('ref_axis',(-0.695179757024368,-0.034691777183374,-0.717998318953046));
#15163=DIRECTION('center_axis',(0.0498412966806708,-0.998757150234825,-1.04083408558608E-17));
#15164=DIRECTION('ref_axis',(-0.695179757024368,-0.034691777183374,-0.717998318953046));
#15165=DIRECTION('center_axis',(0.0498412966806708,-0.998757150234825,-1.04083408558608E-17));
#15166=DIRECTION('ref_axis',(-0.695179757024368,-0.034691777183374,-0.717998318953046));
#15167=DIRECTION('center_axis',(0.0498412966806708,-0.998757150234825,-2.18495763504859E-17));
#15168=DIRECTION('ref_axis',(-0.695179757024368,-0.034691777183374,-0.717998318953046));
#15169=DIRECTION('center_axis',(0.0498412966806708,-0.998757150234825,-2.18495763504859E-17));
#15170=DIRECTION('ref_axis',(0.695179757024366,0.0346917771833739,0.717998318953047));
#15171=DIRECTION('center_axis',(0.0498412966806708,-0.998757150234825,-2.18495763504859E-17));
#15172=DIRECTION('ref_axis',(-0.695179757024368,-0.034691777183374,-0.717998318953046));
#15173=DIRECTION('axis',(0.,0.,1.));
#15174=DIRECTION('refdir',(1.,0.,0.));
#15175=DIRECTION('center_axis',(-0.0498412966806705,0.998757150234825,-3.03153484454085E-17));
#15176=DIRECTION('ref_axis',(-1.51095627584551E-18,3.02776710217119E-17,
1.));
#15177=DIRECTION('center_axis',(-0.0498412966806705,0.998757150234825,-3.03153484454085E-17));
#15178=DIRECTION('ref_axis',(1.51095627584551E-18,-3.02776710217119E-17,
-1.));
#15179=DIRECTION('',(-0.0352431188660326,0.706227953689593,-0.707106781186551));
#15180=DIRECTION('center_axis',(0.0498412966806705,-0.998757150234825,3.03153484454085E-17));
#15181=DIRECTION('ref_axis',(1.51095627584551E-18,-3.02776710217119E-17,
-1.));
#15182=DIRECTION('center_axis',(-8.1583057089881E-17,-6.47172530465054E-17,
-1.));
#15183=DIRECTION('ref_axis',(-0.0498412966806691,0.998757150234825,0.));
#15184=DIRECTION('center_axis',(-8.1583057089881E-17,-6.47172530465054E-17,
-1.));
#15185=DIRECTION('ref_axis',(-0.0498412966806713,0.998757150234825,-6.05706138712209E-17));
#15186=DIRECTION('center_axis',(0.998757150234825,0.0498412966806704,-8.47072534159835E-17));
#15187=DIRECTION('ref_axis',(0.0498412966806704,-0.998757150234825,0.));
#15188=DIRECTION('center_axis',(8.1583057089881E-17,6.47172530465054E-17,
1.));
#15189=DIRECTION('ref_axis',(-0.0498412966806706,0.998757150234825,-6.05706138712209E-17));
#15190=DIRECTION('center_axis',(8.1583057089881E-17,6.47172530465054E-17,
1.));
#15191=DIRECTION('ref_axis',(-0.0498412966806706,0.998757150234825,-6.05706138712209E-17));
#15192=DIRECTION('center_axis',(9.07647421261732E-17,-1.19272213358314E-16,
1.));
#15193=DIRECTION('ref_axis',(0.0498412966806691,-0.998757150234825,0.));
#15194=DIRECTION('center_axis',(9.07647421261732E-17,-1.19272213358314E-16,
1.));
#15195=DIRECTION('ref_axis',(0.0498412966806713,-0.998757150234825,-1.23647808356405E-16));
#15196=DIRECTION('center_axis',(0.998757150234825,0.0498412966806703,-8.47072534159836E-17));
#15197=DIRECTION('ref_axis',(-0.0498412966806703,0.998757150234825,0.));
#15198=DIRECTION('center_axis',(-9.07647421261732E-17,1.19272213358314E-16,
-1.));
#15199=DIRECTION('ref_axis',(0.0498412966806706,-0.998757150234825,-1.23647808356405E-16));
#15200=DIRECTION('center_axis',(-9.07647421261732E-17,1.19272213358314E-16,
-1.));
#15201=DIRECTION('ref_axis',(0.0498412966806706,-0.998757150234825,-1.23647808356405E-16));
#15202=DIRECTION('center_axis',(-8.31133379292631E-17,-3.40523419790356E-17,
-1.));
#15203=DIRECTION('ref_axis',(-0.998757150234825,-0.0498412966806706,8.47072534159836E-17));
#15204=DIRECTION('',(8.31133379292631E-17,3.40523419790356E-17,1.));
#15205=DIRECTION('center_axis',(-0.0498412966806705,0.998757150234825,-1.14936005810131E-16));
#15206=DIRECTION('ref_axis',(-5.728559564874E-18,1.147931576223E-16,1.));
#15207=DIRECTION('center_axis',(0.0498412966806705,-0.998757150234825,1.14936005810131E-16));
#15208=DIRECTION('ref_axis',(5.728559564874E-18,-1.147931576223E-16,-1.));
#15209=DIRECTION('',(-0.0498412966806705,0.998757150234825,-1.14936005810131E-16));
#15210=DIRECTION('center_axis',(0.0498412966806705,-0.998757150234825,1.14936005810131E-16));
#15211=DIRECTION('ref_axis',(5.728559564874E-18,-1.147931576223E-16,-1.));
#15212=DIRECTION('center_axis',(-0.0498412966806705,0.998757150234825,-1.14936005810131E-16));
#15213=DIRECTION('ref_axis',(-5.728559564874E-18,1.147931576223E-16,1.));
#15214=DIRECTION('center_axis',(0.0498412966806705,-0.998757150234825,1.14936005810131E-16));
#15215=DIRECTION('ref_axis',(5.728559564874E-18,-1.147931576223E-16,-1.));
#15216=DIRECTION('',(0.0498412966806705,-0.998757150234825,1.14936005810131E-16));
#15217=DIRECTION('center_axis',(0.0498412966806705,-0.998757150234825,1.14936005810131E-16));
#15218=DIRECTION('ref_axis',(5.728559564874E-18,-1.147931576223E-16,-1.));
#15219=DIRECTION('center_axis',(0.0498412966806705,-0.998757150234825,1.14936005810131E-16));
#15220=DIRECTION('ref_axis',(5.728559564874E-18,-1.147931576223E-16,-1.));
#15221=DIRECTION('center_axis',(-0.0498412966806705,0.998757150234825,-3.03153484454085E-17));
#15222=DIRECTION('ref_axis',(-1.51095627584551E-18,3.02776710217119E-17,
1.));
#15223=DIRECTION('center_axis',(0.0498412966806705,-0.998757150234825,-1.57222324633165E-16));
#15224=DIRECTION('ref_axis',(7.83616452686627E-18,-1.57026920903915E-16,
1.));
#15225=DIRECTION('',(-0.0498412966806705,0.998757150234825,-3.03153484454085E-17));
#15226=DIRECTION('center_axis',(0.0498412966806705,-0.998757150234825,3.03153484454085E-17));
#15227=DIRECTION('ref_axis',(1.51095627584551E-18,-3.02776710217119E-17,
-1.));
#15228=DIRECTION('center_axis',(-0.0498412966806705,0.998757150234825,-3.03153484454085E-17));
#15229=DIRECTION('ref_axis',(-1.51095627584551E-18,3.02776710217119E-17,
1.));
#15230=DIRECTION('center_axis',(-0.0498412966806705,0.998757150234825,8.16022951659984E-17));
#15231=DIRECTION('ref_axis',(4.06716420319217E-18,-8.15008757726136E-17,
1.));
#15232=DIRECTION('',(-0.0498412966806705,0.998757150234825,-3.03153484454085E-17));
#15233=DIRECTION('center_axis',(-8.31133379292631E-17,-3.40523419790356E-17,
-1.));
#15234=DIRECTION('ref_axis',(-0.998757150234825,-0.0498412966806714,8.47072534159836E-17));
#15235=DIRECTION('center_axis',(8.31133379292631E-17,3.40523419790356E-17,
1.));
#15236=DIRECTION('ref_axis',(0.998757150234825,0.0498412966806714,-8.47072534159836E-17));
#15237=DIRECTION('',(-8.31133379292631E-17,-3.40523419790356E-17,-1.));
#15238=DIRECTION('center_axis',(8.31133379292631E-17,3.40523419790356E-17,
1.));
#15239=DIRECTION('ref_axis',(0.998757150234825,0.0498412966806714,-8.47072534159836E-17));
#15240=DIRECTION('center_axis',(-8.31133379292631E-17,-3.40523419790356E-17,
-1.));
#15241=DIRECTION('ref_axis',(-0.998757150234825,-0.0498412966806714,8.47072534159836E-17));
#15242=DIRECTION('center_axis',(8.31133379292631E-17,3.40523419790356E-17,
1.));
#15243=DIRECTION('ref_axis',(0.998757150234825,0.0498412966806714,-8.47072534159836E-17));
#15244=DIRECTION('',(-8.31133379292631E-17,-3.40523419790356E-17,-1.));
#15245=DIRECTION('center_axis',(9.07647421261732E-17,-1.19272213358314E-16,
1.));
#15246=DIRECTION('ref_axis',(0.049841296680668,-0.998757150234825,-1.23647808356404E-16));
#15247=DIRECTION('center_axis',(-8.31133379292631E-17,-3.40523419790356E-17,
-1.));
#15248=DIRECTION('ref_axis',(-0.998757150234825,-0.0498412966806712,8.47072534159835E-17));
#15249=DIRECTION('center_axis',(-8.1583057089881E-17,-6.47172530465054E-17,
-1.));
#15250=DIRECTION('ref_axis',(-0.0498412966806713,0.998757150234825,-6.05706138712209E-17));
#15251=DIRECTION('',(-8.31133379292631E-17,-3.40523419790356E-17,-1.));
#15252=DIRECTION('center_axis',(8.31133379292631E-17,3.40523419790356E-17,
1.));
#15253=DIRECTION('ref_axis',(0.998757150234825,0.0498412966806713,-8.47072534159836E-17));
#15254=DIRECTION('',(-8.31133379292631E-17,-3.40523419790356E-17,-1.));
#15255=DIRECTION('center_axis',(-8.31133379292631E-17,-3.40523419790356E-17,
-1.));
#15256=DIRECTION('ref_axis',(-0.998757150234825,-0.0498412966806714,8.47072534159836E-17));
#15257=DIRECTION('center_axis',(-8.1583057089881E-17,-6.47172530465054E-17,
-1.));
#15258=DIRECTION('ref_axis',(-0.0498412966806681,0.998757150234825,-6.05706138712212E-17));
#15259=DIRECTION('',(-8.31133379292631E-17,-3.40523419790356E-17,-1.));
#15260=DIRECTION('center_axis',(8.31133379292631E-17,3.40523419790356E-17,
1.));
#15261=DIRECTION('ref_axis',(0.998757150234825,0.0498412966806714,-8.47072534159836E-17));
#15262=DIRECTION('center_axis',(-8.31133379292631E-17,-3.40523419790356E-17,
-1.));
#15263=DIRECTION('ref_axis',(-0.998757150234825,-0.0498412966806712,8.47072534159835E-17));
#15264=DIRECTION('center_axis',(8.31133379292631E-17,3.40523419790356E-17,
1.));
#15265=DIRECTION('ref_axis',(0.998757150234825,0.0498412966806713,-8.47072534159836E-17));
#15266=DIRECTION('',(-8.31133379292631E-17,-3.40523419790356E-17,-1.));
#15267=DIRECTION('center_axis',(9.07647421261732E-17,-1.19272213358314E-16,
1.));
#15268=DIRECTION('ref_axis',(0.0498412966806712,-0.998757150234825,-1.23647808356405E-16));
#15269=DIRECTION('',(-8.31133379292631E-17,-3.40523419790356E-17,-1.));
#15270=DIRECTION('center_axis',(0.998757150234825,0.0498412966806707,-7.55063512648625E-17));
#15271=DIRECTION('ref_axis',(-7.54125082139238E-17,-3.76333445466695E-18,
-1.));
#15272=DIRECTION('',(0.998757150234825,0.0498412966806707,-7.55063512648625E-17));
#15273=DIRECTION('center_axis',(0.998757150234825,0.0498412966806707,-7.55063512648625E-17));
#15274=DIRECTION('ref_axis',(-7.54125082139238E-17,-3.76333445466695E-18,
-1.));
#15275=DIRECTION('',(0.998757150234825,0.0498412966806707,-7.55063512648625E-17));
#15276=DIRECTION('center_axis',(0.998757150234825,0.0498412966806708,-7.55063512648625E-17));
#15277=DIRECTION('ref_axis',(-0.0498412966806708,0.998757150234825,-3.22015486701546E-31));
#15278=DIRECTION('',(0.998757150234825,0.0498412966806707,-7.55063512648625E-17));
#15279=DIRECTION('center_axis',(-0.0498412966806705,0.998757150234825,8.20501001114569E-17));
#15280=DIRECTION('ref_axis',(8.86914584083007E-17,-7.772620481529E-17,1.));
#15281=DIRECTION('',(8.86914584083008E-17,-7.772620481529E-17,1.));
#15282=DIRECTION('',(0.998757150234825,0.0498412966806707,-7.55063512648625E-17));
#15283=DIRECTION('center_axis',(0.998757150234825,0.0498412966806707,-7.55063512648625E-17));
#15284=DIRECTION('ref_axis',(-7.54125082139238E-17,-3.76333445466695E-18,
-1.));
#15285=DIRECTION('center_axis',(0.998757150234825,0.0498412966806708,-7.55063512648625E-17));
#15286=DIRECTION('ref_axis',(-0.0498412966806708,0.998757150234825,-3.22015486701546E-31));
#15287=DIRECTION('',(0.998757150234825,0.0498412966806707,-7.55063512648625E-17));
#15288=DIRECTION('center_axis',(0.998757150234825,0.0498412966806707,-7.55063512648625E-17));
#15289=DIRECTION('ref_axis',(-7.54125082139238E-17,-3.76333445466695E-18,
-1.));
#15290=DIRECTION('',(0.998757150234825,0.0498412966806707,-7.55063512648625E-17));
#15291=DIRECTION('center_axis',(0.962724230937995,-0.270484852006255,-6.19392384262883E-17));
#15292=DIRECTION('ref_axis',(0.270484852006255,0.962724230937995,-5.27613511566066E-17));
#15293=DIRECTION('',(0.270484852006255,0.962724230937995,-8.18692862944502E-17));
#15294=DIRECTION('',(-8.31133379292631E-17,-3.40523419790356E-17,-1.));
#15295=DIRECTION('',(-0.270484852006255,-0.962724230937995,5.27613511566066E-17));
#15296=DIRECTION('center_axis',(-0.73203038565962,0.68127198274333,3.09069982706067E-17));
#15297=DIRECTION('ref_axis',(-0.68127198274333,-0.73203038565962,7.52661071837786E-17));
#15298=DIRECTION('',(0.68127198274333,0.73203038565962,-7.52661071837786E-17));
#15299=DIRECTION('',(8.31133379292631E-17,3.40523419790356E-17,1.));
#15300=DIRECTION('',(-0.68127198274333,-0.73203038565962,9.66712163971166E-17));
#15301=DIRECTION('center_axis',(7.39238711172199E-17,3.35937570851917E-17,
1.));
#15302=DIRECTION('ref_axis',(0.998757150234825,0.0498412966806707,-7.55063512648625E-17));
#15303=DIRECTION('',(0.68127198274333,0.73203038565962,-7.52661071837786E-17));
#15304=DIRECTION('center_axis',(8.31133379292631E-17,3.40523419790356E-17,
1.));
#15305=DIRECTION('ref_axis',(0.998757150234825,0.0498412966806708,-8.47072534159836E-17));
#15306=DIRECTION('',(-0.0498412966806705,0.998757150234825,-3.03153484454085E-17));
#15307=DIRECTION('',(-0.998757150234825,-0.0498412966806707,7.55063512648625E-17));
#15308=DIRECTION('',(0.0498412966806706,-0.998757150234825,3.03153484454085E-17));
#15309=DIRECTION('center_axis',(-8.31133379292631E-17,-3.40523419790356E-17,
-1.));
#15310=DIRECTION('ref_axis',(0.998757150234825,0.0498412966806708,-8.47072534159836E-17));
#15311=DIRECTION('',(-0.270484852006255,-0.962724230937995,5.27613511566066E-17));
#15312=DIRECTION('center_axis',(7.39238711172199E-17,3.35937570851917E-17,
1.));
#15313=DIRECTION('ref_axis',(0.998757150234825,0.0498412966806707,-7.55063512648625E-17));
#15314=DIRECTION('',(-0.0498412966806705,0.998757150234825,-3.03153484454085E-17));
#15315=DIRECTION('center_axis',(-8.31133379292631E-17,-3.40523419790356E-17,
-1.));
#15316=DIRECTION('ref_axis',(0.998757150234825,0.0498412966806708,-8.47072534159836E-17));
#15317=DIRECTION('center_axis',(8.31133379292631E-17,3.40523419790356E-17,
1.));
#15318=DIRECTION('ref_axis',(0.998757150234825,0.0498412966806708,-8.47072534159836E-17));
#15319=DIRECTION('',(0.0498412966806706,-0.998757150234825,3.03153484454085E-17));
#15320=DIRECTION('',(0.998757150234825,0.0498412966806707,-7.55063512648625E-17));
#15321=DIRECTION('center_axis',(0.0498412966806705,-0.998757150234825,2.986754349995E-17));
#15322=DIRECTION('ref_axis',(-8.31133379292631E-17,-3.40523419790355E-17,
-1.));
#15323=DIRECTION('',(-8.31133379292631E-17,-3.40523419790356E-17,-1.));
#15324=DIRECTION('',(-0.998757150234825,-0.0498412966806707,7.55063512648625E-17));
#15325=DIRECTION('',(-8.31133379292631E-17,-3.40523419790356E-17,-1.));
#15326=DIRECTION('',(0.998757150234825,0.0498412966806707,-7.55063512648625E-17));
#15327=DIRECTION('center_axis',(0.998757150234825,0.0498412966806706,-7.55063512648625E-17));
#15328=DIRECTION('ref_axis',(-0.0498412966806706,0.998757150234825,-3.03153484454085E-17));
#15329=DIRECTION('',(0.0498412966806706,-0.998757150234825,-1.23200003410946E-16));
#15330=DIRECTION('',(8.31133379292631E-17,3.40523419790356E-17,1.));
#15331=DIRECTION('center_axis',(-0.998757150234825,-0.0498412966806708,
7.55063512648625E-17));
#15332=DIRECTION('ref_axis',(-0.0498412966806708,0.998757150234825,2.19556013660145E-31));
#15333=DIRECTION('center_axis',(-0.998757150234825,-0.0498412966806708,
7.55063512648625E-17));
#15334=DIRECTION('ref_axis',(-0.0498412966806708,0.998757150234825,2.19556013660145E-31));
#15335=DIRECTION('',(8.31133379292631E-17,3.40523419790356E-17,1.));
#15336=DIRECTION('',(-0.0498412966806706,0.998757150234825,-6.10184188166794E-17));
#15337=DIRECTION('',(9.24604587319749E-17,-1.53252249946591E-16,1.));
#15338=DIRECTION('',(0.0498412966806706,-0.998757150234825,-1.43156999152272E-16));
#15339=DIRECTION('',(-8.31133379292631E-17,-3.40523419790356E-17,-1.));
#15340=DIRECTION('',(-0.0498412966806706,0.998757150234825,-3.03153484454085E-17));
#15341=DIRECTION('center_axis',(0.962724230937995,-0.270484852006255,-6.19392384262883E-17));
#15342=DIRECTION('ref_axis',(0.270484852006255,0.962724230937995,-5.27613511566066E-17));
#15343=DIRECTION('',(-8.31133379292631E-17,-3.40523419790356E-17,-1.));
#15344=DIRECTION('',(-0.270484852006255,-0.962724230937995,-9.27783245326118E-17));
#15345=DIRECTION('center_axis',(-0.73203038565962,0.68127198274333,3.09069982706067E-17));
#15346=DIRECTION('ref_axis',(-0.68127198274333,-0.73203038565962,7.52661071837786E-17));
#15347=DIRECTION('',(0.68127198274333,0.73203038565962,3.17594388829113E-17));
#15348=DIRECTION('',(8.31133379292631E-17,3.40523419790356E-17,1.));
#15349=DIRECTION('center_axis',(-0.998757150234825,-0.0498412966806707,
8.47072534159836E-17));
#15350=DIRECTION('ref_axis',(8.31133379292631E-17,3.40523419790356E-17,
1.));
#15351=DIRECTION('',(-0.0498412966806705,0.998757150234825,-6.10184188166794E-17));
#15352=DIRECTION('',(-8.31133379292631E-17,-3.40523419790356E-17,-1.));
#15353=DIRECTION('center_axis',(0.998757150234825,0.0498412966806707,-7.55063512648625E-17));
#15354=DIRECTION('ref_axis',(7.54125082139238E-17,3.76333445466695E-18,
1.));
#15355=DIRECTION('center_axis',(0.998757150234825,0.0498412966806707,-7.55063512648625E-17));
#15356=DIRECTION('ref_axis',(7.54125082139238E-17,3.76333445466695E-18,
1.));
#15357=DIRECTION('',(-8.31133379292631E-17,-3.40523419790356E-17,-1.));
#15358=DIRECTION('',(0.0498412966806705,-0.998757150234825,-1.23200003410946E-16));
#15359=DIRECTION('',(9.24604587319749E-17,-1.53252249946591E-16,1.));
#15360=DIRECTION('',(-0.0498412966806705,0.998757150234825,-3.03153484454085E-17));
#15361=DIRECTION('',(-8.31133379292631E-17,-3.40523419790356E-17,-1.));
#15362=DIRECTION('',(0.0498412966806705,-0.998757150234825,-1.43156999152272E-16));
#15363=DIRECTION('',(8.86914584083008E-17,-7.772620481529E-17,1.));
#15364=DIRECTION('center_axis',(-0.998757150234825,-0.0498412966806707,
7.55063512648625E-17));
#15365=DIRECTION('ref_axis',(7.54125082139238E-17,3.76333445466695E-18,
1.));
#15366=DIRECTION('center_axis',(0.998757150234825,0.0498412966806707,-7.55063512648625E-17));
#15367=DIRECTION('ref_axis',(-7.54125082139238E-17,-3.76333445466695E-18,
-1.));
#15368=DIRECTION('center_axis',(-0.0498412966806705,0.998757150234825,1.57670129578624E-16));
#15369=DIRECTION('ref_axis',(9.24604587319748E-17,-1.53252249946591E-16,
1.));
#15370=DIRECTION('',(0.998757150234825,0.0498412966806707,-7.55063512648625E-17));
#15371=DIRECTION('',(0.998757150234825,0.0498412966806707,-7.55063512648625E-17));
#15372=DIRECTION('center_axis',(-8.15607379107394E-17,-6.51645014376925E-17,
-1.));
#15373=DIRECTION('ref_axis',(-0.0498412966806705,0.998757150234825,-6.10184188166794E-17));
#15374=DIRECTION('center_axis',(8.1583057089881E-17,6.47172530465054E-17,
1.));
#15375=DIRECTION('ref_axis',(-0.0498412966806736,0.998757150234825,-6.05706138712207E-17));
#15376=DIRECTION('center_axis',(-8.1583057089881E-17,-6.47172530465054E-17,
-1.));
#15377=DIRECTION('ref_axis',(-0.0498412966806694,0.998757150234825,-6.05706138712211E-17));
#15378=DIRECTION('center_axis',(9.07424229470315E-17,-1.18824964967127E-16,
1.));
#15379=DIRECTION('ref_axis',(0.0498412966806705,-0.998757150234825,-1.23200003410946E-16));
#15380=DIRECTION('center_axis',(-9.07647421261732E-17,1.19272213358314E-16,
-1.));
#15381=DIRECTION('ref_axis',(0.0498412966806736,-0.998757150234825,-1.23647808356405E-16));
#15382=DIRECTION('center_axis',(9.07647421261732E-17,-1.19272213358314E-16,
1.));
#15383=DIRECTION('ref_axis',(0.0498412966806694,-0.998757150234825,-1.23647808356405E-16));
#15384=DIRECTION('center_axis',(0.0498412966806705,-0.998757150234825,2.986754349995E-17));
#15385=DIRECTION('ref_axis',(-8.31133379292631E-17,-3.40523419790355E-17,
-1.));
#15386=DIRECTION('',(0.998757150234825,0.0498412966806707,-7.55063512648625E-17));
#15387=DIRECTION('',(0.998757150234825,0.0498412966806707,-7.55063512648625E-17));
#15388=DIRECTION('center_axis',(9.17371054926298E-17,-1.38757157160982E-16,
1.));
#15389=DIRECTION('ref_axis',(0.0498412966806705,-0.998757150234825,-1.43156999152272E-16));
#15390=DIRECTION('center_axis',(-0.0498412966806705,0.998757150234825,8.20501001114569E-17));
#15391=DIRECTION('ref_axis',(8.86914584083007E-17,-7.772620481529E-17,1.));
#15392=DIRECTION('center_axis',(-7.39238711172199E-17,-3.35937570851917E-17,
-1.));
#15393=DIRECTION('ref_axis',(-0.998757150234825,-0.0498412966806707,7.55063512648625E-17));
#15394=DIRECTION('center_axis',(0.0498412966806705,-0.998757150234825,1.14488200864672E-16));
#15395=DIRECTION('ref_axis',(-7.88957346402346E-17,-1.18567828579623E-16,
-1.));
#15396=DIRECTION('center_axis',(0.0498412966806705,-0.998757150234825,1.14488200864672E-16));
#15397=DIRECTION('ref_axis',(-7.88957346402346E-17,-1.18567828579623E-16,
-1.));
#15398=DIRECTION('center_axis',(8.31133379292631E-17,3.40523419790356E-17,
1.));
#15399=DIRECTION('ref_axis',(0.998757150234825,0.0498412966806708,-8.47072534159836E-17));
#15400=DIRECTION('center_axis',(8.31133379292631E-17,3.40523419790356E-17,
1.));
#15401=DIRECTION('ref_axis',(0.998757150234825,0.0498412966806708,-8.47072534159836E-17));
#15402=DIRECTION('center_axis',(-8.31133379292631E-17,-3.40523419790356E-17,
-1.));
#15403=DIRECTION('ref_axis',(-0.998757150234825,-0.0498412966806708,8.47072534159836E-17));
#15404=DIRECTION('center_axis',(-8.31133379292631E-17,-3.40523419790356E-17,
-1.));
#15405=DIRECTION('ref_axis',(-0.998757150234825,-0.0498412966806708,8.47072534159836E-17));
#15406=DIRECTION('axis',(0.,0.,1.));
#15407=DIRECTION('refdir',(1.,0.,0.));
#15408=DIRECTION('center_axis',(0.,0.,-1.));
#15409=DIRECTION('ref_axis',(-0.99771030462832,0.067632448118233,0.));
#15410=DIRECTION('center_axis',(0.,0.,-1.));
#15411=DIRECTION('ref_axis',(0.99771030462832,-0.0676324481182314,0.));
#15412=DIRECTION('',(-0.705487722062377,0.0478233626926498,0.707106781186551));
#15413=DIRECTION('center_axis',(0.,0.,1.));
#15414=DIRECTION('ref_axis',(0.99771030462832,-0.067632448118233,0.));
#15415=DIRECTION('center_axis',(0.,0.,1.));
#15416=DIRECTION('ref_axis',(0.99771030462832,-0.0676324481182314,0.));
#15417=DIRECTION('center_axis',(0.,0.,1.));
#15418=DIRECTION('ref_axis',(0.99771030462832,-0.0676324481182314,0.));
#15419=DIRECTION('center_axis',(0.,0.,1.));
#15420=DIRECTION('ref_axis',(0.99771030462832,-0.0676324481182314,0.));
#15421=DIRECTION('',(0.705487722062381,-0.0478233626926487,-0.707106781186547));
#15422=DIRECTION('center_axis',(0.,0.,-1.));
#15423=DIRECTION('ref_axis',(0.99771030462832,-0.0676324481182291,0.));
#15424=DIRECTION('center_axis',(0.,0.,-1.));
#15425=DIRECTION('ref_axis',(-0.99771030462832,0.0676324481182314,0.));
#15426=DIRECTION('',(0.,0.,1.));
#15427=DIRECTION('center_axis',(0.,0.,1.));
#15428=DIRECTION('ref_axis',(0.99771030462832,-0.0676324481182317,0.));
#15429=DIRECTION('center_axis',(0.,0.,1.));
#15430=DIRECTION('ref_axis',(0.99771030462832,-0.0676324481182317,0.));
#15431=DIRECTION('center_axis',(0.,0.,-1.));
#15432=DIRECTION('ref_axis',(-0.999999893830928,0.00046080162076951,0.));
#15433=DIRECTION('center_axis',(0.,0.,-1.));
#15434=DIRECTION('ref_axis',(0.999999893830927,-0.000460801620770501,0.));
#15435=DIRECTION('',(-0.707106706113674,0.000325835950827958,0.70710678118655));
#15436=DIRECTION('center_axis',(0.,0.,1.));
#15437=DIRECTION('ref_axis',(0.999999893830928,-0.00046080162076951,0.));
#15438=DIRECTION('center_axis',(0.,0.,1.));
#15439=DIRECTION('ref_axis',(0.999999893830927,-0.000460801620770501,0.));
#15440=DIRECTION('center_axis',(0.,0.,1.));
#15441=DIRECTION('ref_axis',(0.999999893830927,-0.000460801620770501,0.));
#15442=DIRECTION('center_axis',(0.,0.,1.));
#15443=DIRECTION('ref_axis',(0.999999893830927,-0.000460801620770501,0.));
#15444=DIRECTION('',(0.707106706113681,-0.000325835950828489,-0.707106781186542));
#15445=DIRECTION('center_axis',(0.,0.,-1.));
#15446=DIRECTION('ref_axis',(0.999999893830928,-0.00046080162076951,0.));
#15447=DIRECTION('center_axis',(0.,0.,-1.));
#15448=DIRECTION('ref_axis',(-0.999999893830927,0.000460801620770501,0.));
#15449=DIRECTION('',(0.,0.,1.));
#15450=DIRECTION('center_axis',(0.,0.,1.));
#15451=DIRECTION('ref_axis',(0.999999893830928,-0.00046080162077021,0.));
#15452=DIRECTION('center_axis',(0.,0.,1.));
#15453=DIRECTION('ref_axis',(0.999999893830928,-0.00046080162077021,0.));
#15454=DIRECTION('',(0.,0.,1.));
#15455=DIRECTION('',(1.,0.,0.));
#15456=DIRECTION('',(0.,0.,1.));
#15457=DIRECTION('',(1.,0.,0.));
#15458=DIRECTION('',(0.,0.,1.));
#15459=DIRECTION('',(1.,0.,0.));
#15460=DIRECTION('axis',(0.,0.,1.));
#15461=DIRECTION('refdir',(1.,0.,0.));
#15462=DIRECTION('center_axis',(1.34374111916937E-16,-6.5016645363134E-17,
1.));
#15463=DIRECTION('ref_axis',(0.997400584683992,-0.0720560453538152,-1.38709660139384E-16));
#15464=DIRECTION('center_axis',(-1.34374111916937E-16,6.5016645363134E-17,
-1.));
#15465=DIRECTION('ref_axis',(-0.997400584683992,0.0720560453538154,1.38709660139384E-16));
#15466=DIRECTION('',(1.34374111916937E-16,-6.5016645363134E-17,1.));
#15467=DIRECTION('center_axis',(-1.34374111916937E-16,6.5016645363134E-17,
-1.));
#15468=DIRECTION('ref_axis',(-0.997400584683992,0.0720560453538154,1.38709660139384E-16));
#15469=DIRECTION('center_axis',(1.34374111916937E-16,-6.5016645363134E-17,
1.));
#15470=DIRECTION('ref_axis',(0.997400584683992,-0.0720560453538153,-1.38709660139384E-16));
#15471=DIRECTION('center_axis',(-1.34374111916937E-16,6.5016645363134E-17,
-1.));
#15472=DIRECTION('ref_axis',(-0.997400584683992,0.0720560453538153,1.38709660139384E-16));
#15473=DIRECTION('',(1.34374111916937E-16,-6.5016645363134E-17,1.));
#15474=DIRECTION('center_axis',(-1.34374111916937E-16,6.5016645363134E-17,
-1.));
#15475=DIRECTION('ref_axis',(-0.997400584683992,0.0720560453538153,1.38709660139384E-16));
#15476=DIRECTION('center_axis',(-9.47320768979473E-17,6.21527526432887E-17,
-1.));
#15477=DIRECTION('ref_axis',(-0.997400584683992,0.072056045353816,9.89643104496708E-17));
#15478=DIRECTION('',(-0.997400584683992,0.072056045353816,9.89643104496708E-17));
#15479=DIRECTION('center_axis',(-1.34374111916937E-16,6.5016645363134E-17,
-1.));
#15480=DIRECTION('ref_axis',(-0.997400584683992,0.0720560453538159,1.38709660139384E-16));
#15481=DIRECTION('',(0.0720560453538158,0.997400584683992,6.43240143985008E-17));
#15482=DIRECTION('center_axis',(-1.34374111916937E-16,6.5016645363134E-17,
-1.));
#15483=DIRECTION('ref_axis',(-0.997400584683992,0.0720560453538159,1.38709660139384E-16));
#15484=DIRECTION('',(0.997400584683992,-0.072056045353816,-9.89643104496708E-17));
#15485=DIRECTION('center_axis',(-1.34374111916937E-16,6.5016645363134E-17,
-1.));
#15486=DIRECTION('ref_axis',(-0.997400584683992,0.072056045353816,1.38709660139384E-16));
#15487=DIRECTION('',(-0.0720560453538158,-0.997400584683992,-6.43240143985008E-17));
#15488=DIRECTION('center_axis',(-1.34374111916937E-16,6.5016645363134E-17,
-1.));
#15489=DIRECTION('ref_axis',(-0.997400584683992,0.072056045353816,1.38709660139384E-16));
#15490=DIRECTION('center_axis',(-9.47320768979473E-17,6.21527526432887E-17,
-1.));
#15491=DIRECTION('ref_axis',(-0.997400584683992,0.072056045353816,9.89643104496708E-17));
#15492=DIRECTION('',(0.0720560453538158,0.997400584683992,6.43240143985008E-17));
#15493=DIRECTION('center_axis',(1.34374111916937E-16,-6.5016645363134E-17,
1.));
#15494=DIRECTION('ref_axis',(-0.997400584683992,0.0720560453538159,1.38709660139384E-16));
#15495=DIRECTION('',(-0.997400584683992,0.072056045353816,9.89643104496708E-17));
#15496=DIRECTION('center_axis',(1.34374111916937E-16,-6.5016645363134E-17,
1.));
#15497=DIRECTION('ref_axis',(-0.997400584683992,0.0720560453538174,1.38709660139384E-16));
#15498=DIRECTION('',(-0.0720560453538158,-0.997400584683992,-6.43240143985008E-17));
#15499=DIRECTION('center_axis',(1.34374111916937E-16,-6.5016645363134E-17,
1.));
#15500=DIRECTION('ref_axis',(-0.997400584683992,0.072056045353816,1.38709660139384E-16));
#15501=DIRECTION('',(0.997400584683992,-0.072056045353816,-9.89643104496708E-17));
#15502=DIRECTION('center_axis',(1.34374111916937E-16,-6.5016645363134E-17,
1.));
#15503=DIRECTION('ref_axis',(-0.997400584683992,0.0720560453538076,1.38709660139383E-16));
#15504=DIRECTION('center_axis',(0.997400584683992,-0.0720560453538159,-1.38709660139384E-16));
#15505=DIRECTION('ref_axis',(-1.34374111916937E-16,6.5016645363134E-17,
-1.));
#15506=DIRECTION('',(1.34374111916937E-16,-6.5016645363134E-17,1.));
#15507=DIRECTION('',(-1.34374111916937E-16,6.5016645363134E-17,-1.));
#15508=DIRECTION('center_axis',(-0.0720560453538158,-0.997400584683992,
-5.51651729967161E-17));
#15509=DIRECTION('ref_axis',(1.34374111916937E-16,-6.5016645363134E-17,
1.));
#15510=DIRECTION('',(1.34374111916937E-16,-6.5016645363134E-17,1.));
#15511=DIRECTION('',(-1.34374111916937E-16,6.5016645363134E-17,-1.));
#15512=DIRECTION('center_axis',(-0.997400584683992,0.0720560453538159,1.38709660139384E-16));
#15513=DIRECTION('ref_axis',(1.34374111916937E-16,-6.5016645363134E-17,
1.));
#15514=DIRECTION('',(-1.34374111916937E-16,6.5016645363134E-17,-1.));
#15515=DIRECTION('',(1.34374111916937E-16,-6.5016645363134E-17,1.));
#15516=DIRECTION('center_axis',(0.0720560453538158,0.997400584683992,5.51651729967161E-17));
#15517=DIRECTION('ref_axis',(-1.34374111916937E-16,6.5016645363134E-17,
-1.));
#15518=DIRECTION('',(-1.34374111916937E-16,6.5016645363134E-17,-1.));
#15519=DIRECTION('',(1.34374111916937E-16,-6.5016645363134E-17,1.));
#15520=DIRECTION('center_axis',(1.34374111916937E-16,-6.5016645363134E-17,
1.));
#15521=DIRECTION('ref_axis',(0.997400584683992,-0.0720560453538159,-1.38709660139384E-16));
#15522=DIRECTION('center_axis',(1.34374111916937E-16,-6.5016645363134E-17,
1.));
#15523=DIRECTION('ref_axis',(0.997400584683992,-0.0720560453538161,-1.38709660139384E-16));
#15524=DIRECTION('center_axis',(1.34374111916937E-16,-6.5016645363134E-17,
1.));
#15525=DIRECTION('ref_axis',(0.997400584683992,-0.072056045353816,-1.38709660139384E-16));
#15526=DIRECTION('center_axis',(1.34374111916937E-16,-6.5016645363134E-17,
1.));
#15527=DIRECTION('ref_axis',(0.997400584683992,-0.072056045353816,-1.38709660139384E-16));
#15528=DIRECTION('axis',(0.,0.,1.));
#15529=DIRECTION('refdir',(1.,0.,0.));
#15530=DIRECTION('axis',(0.,0.,1.));
#15531=DIRECTION('refdir',(1.,0.,0.));
#15532=DIRECTION('center_axis',(-0.974431531646231,0.224684645967589,-1.26428912495664E-17));
#15533=DIRECTION('ref_axis',(-1.23196318847518E-17,2.84066354441556E-18,
1.));
#15534=DIRECTION('',(-0.974431531646231,0.224684645967589,-1.26428912495664E-17));
#15535=DIRECTION('center_axis',(-0.974431531646231,0.224684645967589,-1.26428912495664E-17));
#15536=DIRECTION('ref_axis',(-1.23196318847518E-17,2.84066354441556E-18,
1.));
#15537=DIRECTION('center_axis',(2.08745462991212E-17,1.24347063228184E-16,
-1.));
#15538=DIRECTION('ref_axis',(-0.974431531646231,0.22468464596759,0.));
#15539=DIRECTION('center_axis',(2.08745462991212E-17,1.24347063228184E-16,
-1.));
#15540=DIRECTION('ref_axis',(-0.974431531646231,0.224684645967589,7.59805975586113E-18));
#15541=DIRECTION('center_axis',(-0.224684645967589,-0.974431531646231,-1.25857889322102E-16));
#15542=DIRECTION('ref_axis',(0.974431531646231,-0.224684645967589,0.));
#15543=DIRECTION('center_axis',(-2.08745462991212E-17,-1.24347063228184E-16,
1.));
#15544=DIRECTION('ref_axis',(-0.974431531646231,0.224684645967589,7.59805975586113E-18));
#15545=DIRECTION('center_axis',(-2.08745462991212E-17,-1.24347063228184E-16,
1.));
#15546=DIRECTION('ref_axis',(-0.974431531646231,0.224684645967589,7.59805975586113E-18));
#15547=DIRECTION('center_axis',(2.08745462991212E-17,1.24347063228184E-16,
-1.));
#15548=DIRECTION('ref_axis',(-0.974431531646231,0.22468464596759,0.));
#15549=DIRECTION('center_axis',(2.08745462991212E-17,1.24347063228184E-16,
-1.));
#15550=DIRECTION('ref_axis',(-0.974431531646231,0.224684645967589,7.59805975586113E-18));
#15551=DIRECTION('center_axis',(2.08745462991212E-17,1.24347063228184E-16,
-1.));
#15552=DIRECTION('ref_axis',(-0.974431531646231,0.224684645967589,7.59805975586113E-18));
#15553=DIRECTION('center_axis',(-0.224684645967589,-0.974431531646231,-1.25857889322102E-16));
#15554=DIRECTION('ref_axis',(0.974431531646231,-0.224684645967589,0.));
#15555=DIRECTION('center_axis',(-2.08745462991212E-17,-1.24347063228184E-16,
1.));
#15556=DIRECTION('ref_axis',(-0.974431531646231,0.224684645967589,7.59805975586113E-18));
#15557=DIRECTION('center_axis',(-0.974431531646231,0.224684645967589,-1.26428912495664E-17));
#15558=DIRECTION('ref_axis',(-1.23196318847518E-17,2.84066354441556E-18,
1.));
#15559=DIRECTION('center_axis',(-0.974431531646231,0.224684645967589,-1.26428912495664E-17));
#15560=DIRECTION('ref_axis',(-1.23196318847518E-17,2.84066354441556E-18,
1.));
#15561=DIRECTION('',(-0.974431531646231,0.224684645967589,-1.26428912495664E-17));
#15562=DIRECTION('center_axis',(-0.974431531646231,0.224684645967589,-1.26428912495664E-17));
#15563=DIRECTION('ref_axis',(-1.23196318847518E-17,2.84066354441556E-18,
1.));
#15564=DIRECTION('center_axis',(0.224684645967589,0.974431531646231,6.60780807231409E-17));
#15565=DIRECTION('ref_axis',(1.48467301734967E-17,6.43885654072935E-17,
-1.));
#15566=DIRECTION('center_axis',(0.224684645967589,0.974431531646231,6.60780807231409E-17));
#15567=DIRECTION('ref_axis',(1.48467301734967E-17,6.43885654072935E-17,
-1.));
#15568=DIRECTION('',(0.224684645967589,0.974431531646231,6.60780807231409E-17));
#15569=DIRECTION('center_axis',(0.224684645967589,0.974431531646231,6.60780807231409E-17));
#15570=DIRECTION('ref_axis',(1.48467301734967E-17,6.43885654072935E-17,
-1.));
#15571=DIRECTION('center_axis',(2.08745462991212E-17,1.24347063228184E-16,
-1.));
#15572=DIRECTION('ref_axis',(-0.974431531646231,0.224684645967588,7.59805975586093E-18));
#15573=DIRECTION('center_axis',(2.08745462991212E-17,1.24347063228184E-16,
-1.));
#15574=DIRECTION('ref_axis',(-0.974431531646231,0.224684645967588,7.59805975586093E-18));
#15575=DIRECTION('',(2.08745462991212E-17,1.24347063228184E-16,-1.));
#15576=DIRECTION('center_axis',(2.08745462991212E-17,1.24347063228184E-16,
-1.));
#15577=DIRECTION('ref_axis',(-0.974431531646231,0.224684645967588,7.59805975586093E-18));
#15578=DIRECTION('center_axis',(2.08745462991212E-17,1.24347063228184E-16,
-1.));
#15579=DIRECTION('ref_axis',(-0.974431531646231,0.224684645967589,7.59805975586113E-18));
#15580=DIRECTION('center_axis',(2.08745462991212E-17,1.24347063228184E-16,
-1.));
#15581=DIRECTION('ref_axis',(-0.974431531646231,0.224684645967589,7.59805975586113E-18));
#15582=DIRECTION('',(2.08745462991212E-17,1.24347063228184E-16,-1.));
#15583=DIRECTION('center_axis',(2.08745462991212E-17,1.24347063228184E-16,
-1.));
#15584=DIRECTION('ref_axis',(-0.974431531646231,0.224684645967589,7.59805975586113E-18));
#15585=DIRECTION('center_axis',(-0.147090628234403,-0.637915179045802,0.755928946018455));
#15586=DIRECTION('ref_axis',(0.169845627612808,0.736601000684484,0.654653670707977));
#15587=DIRECTION('center_axis',(0.224684645967553,0.974431531646239,-1.2074073682481E-13));
#15588=DIRECTION('ref_axis',(-2.27979080437047E-11,5.38065576097235E-12,
1.));
#15589=DIRECTION('center_axis',(-0.843882460965992,0.194582612535136,-0.499999998972983));
#15590=DIRECTION('ref_axis',(0.50338836685051,0.609594266156192,-0.612368339146523));
#15591=DIRECTION('',(0.147090628234403,0.637915179045802,-0.755928946018455));
#15592=DIRECTION('center_axis',(-0.48721576582319,0.112342322983636,0.866025403784417));
#15593=DIRECTION('ref_axis',(0.227358619108416,-0.941173766267205,0.250000000015036));
#15594=DIRECTION('center_axis',(0.487215765823101,-0.11234232298411,0.866025403784406));
#15595=DIRECTION('ref_axis',(-0.616523841550484,-0.746591155056556,0.249999999982304));
#15596=DIRECTION('',(-0.147090628234403,-0.637915179045802,0.755928946018454));
#15597=DIRECTION('center_axis',(-0.843882461168241,0.19458261062525,0.499999999374895));
#15598=DIRECTION('ref_axis',(0.185637904156542,-0.768464715336596,0.612372884624238));
#15599=DIRECTION('center_axis',(0.147090628234407,0.637915179045802,0.755928946018454));
#15600=DIRECTION('ref_axis',(0.169845627612808,0.736601000684483,-0.654653670707978));
#15601=DIRECTION('center_axis',(0.487215765823114,-0.112342322983753,-0.866025403784445));
#15602=DIRECTION('ref_axis',(0.616523841554425,0.746591155052271,0.249999999985382));
#15603=DIRECTION('center_axis',(-0.487215765823237,0.11234232298353,-0.866025403784404));
#15604=DIRECTION('ref_axis',(-0.227358619080957,0.94117376627761,0.250000000000839));
#15605=DIRECTION('',(-0.147090628234407,-0.637915179045802,-0.755928946018454));
#15606=DIRECTION('center_axis',(-0.843882459372318,0.194582605937149,0.500000004230436));
#15607=DIRECTION('ref_axis',(0.503389000994448,0.60959164109859,0.612370431014218));
#15608=DIRECTION('center_axis',(0.224684645967565,0.974431531646236,6.66256114045275E-14));
#15609=DIRECTION('ref_axis',(6.59444949636519E-12,-1.58892350212702E-12,
1.));
#15610=DIRECTION('center_axis',(-0.843882462501695,0.194582609008347,-0.499999997753581));
#15611=DIRECTION('ref_axis',(-0.18563903427446,0.768463346797486,0.612374259405515));
#15612=DIRECTION('',(0.147090628234407,0.637915179045802,0.755928946018454));
#15613=DIRECTION('center_axis',(-0.224684645967589,-0.974431531646231,-6.60780807231409E-17));
#15614=DIRECTION('ref_axis',(-0.974431531646231,0.224684645967589,-3.69778549322349E-32));
#15615=DIRECTION('center_axis',(0.224684645967589,0.974431531646231,6.60780807231409E-17));
#15616=DIRECTION('ref_axis',(-0.974431531646231,0.224684645967589,-3.69778549322349E-32));
#15617=DIRECTION('',(0.224684645967589,0.974431531646231,6.60780807231409E-17));
#15618=DIRECTION('center_axis',(0.224684645967589,0.974431531646231,6.60780807231409E-17));
#15619=DIRECTION('ref_axis',(0.974431531646231,-0.224684645967589,3.69778549322349E-32));
#15620=DIRECTION('center_axis',(0.224684645967589,0.974431531646231,6.60780807231409E-17));
#15621=DIRECTION('ref_axis',(0.974431531646231,-0.224684645967589,3.69778549322349E-32));
#15622=DIRECTION('center_axis',(0.224684645967589,0.974431531646231,6.60780807231409E-17));
#15623=DIRECTION('ref_axis',(0.974431531646231,-0.224684645967589,3.69778549322349E-32));
#15624=DIRECTION('center_axis',(0.224684645967589,0.974431531646231,6.60780807231409E-17));
#15625=DIRECTION('ref_axis',(0.974431531646231,-0.224684645967589,3.69778549322349E-32));
#15626=DIRECTION('center_axis',(0.224684645967589,0.974431531646231,6.60780807231409E-17));
#15627=DIRECTION('ref_axis',(0.974431531646231,-0.224684645967589,3.69778549322349E-32));
#15628=DIRECTION('center_axis',(0.224684645967589,0.974431531646231,6.60780807231409E-17));
#15629=DIRECTION('ref_axis',(0.974431531646231,-0.224684645967589,3.69778549322349E-32));
#15630=DIRECTION('center_axis',(9.84588993227597E-17,-1.5186299647836E-16,
1.));
#15631=DIRECTION('ref_axis',(0.974431531646231,-0.224684645967587,-1.30062739670596E-16));
#15632=DIRECTION('center_axis',(8.84893164462714E-17,1.08756434026123E-16,
-1.));
#15633=DIRECTION('ref_axis',(0.974431531646231,-0.22468464596759,6.17908792832111E-17));
#15634=DIRECTION('',(-9.84588993227597E-17,1.5186299647836E-16,-1.));
#15635=DIRECTION('center_axis',(-2.08745462991212E-17,-1.24347063228184E-16,
1.));
#15636=DIRECTION('ref_axis',(-0.974431531646223,0.224684645967624,7.59805975586562E-18));
#15637=DIRECTION('',(9.84588993227597E-17,-1.5186299647836E-16,1.));
#15638=DIRECTION('center_axis',(-0.974431531646231,0.224684645967589,-1.26428912495664E-17));
#15639=DIRECTION('ref_axis',(0.224684645967589,0.974431531646231,-2.31111593326468E-33));
#15640=DIRECTION('center_axis',(-0.974431531646231,0.224684645967589,-1.26428912495664E-17));
#15641=DIRECTION('ref_axis',(0.224684645967589,0.974431531646231,-2.31111593326468E-33));
#15642=DIRECTION('',(0.974431531646231,-0.224684645967589,1.26428912495664E-17));
#15643=DIRECTION('center_axis',(-0.974431531646231,0.224684645967589,-1.26428912495664E-17));
#15644=DIRECTION('ref_axis',(0.224684645967589,0.974431531646231,-2.31111593326468E-33));
#15645=DIRECTION('center_axis',(-0.974431531646231,0.224684645967589,-1.26428912495664E-17));
#15646=DIRECTION('ref_axis',(0.224684645967589,0.974431531646231,-2.69630192214213E-33));
#15647=DIRECTION('center_axis',(-0.974431531646231,0.224684645967589,-1.26428912495664E-17));
#15648=DIRECTION('ref_axis',(0.224684645967589,0.974431531646231,-2.69630192214213E-33));
#15649=DIRECTION('',(0.974431531646231,-0.224684645967589,1.26428912495664E-17));
#15650=DIRECTION('center_axis',(-0.974431531646231,0.224684645967589,-1.26428912495664E-17));
#15651=DIRECTION('ref_axis',(0.224684645967589,0.974431531646231,-2.69630192214213E-33));
#15652=DIRECTION('center_axis',(-0.974431531646231,0.224684645967589,-1.26428912495664E-17));
#15653=DIRECTION('ref_axis',(0.224684645967589,0.974431531646231,-2.31111593326468E-33));
#15654=DIRECTION('center_axis',(-0.974431531646231,0.224684645967589,-1.26428912495664E-17));
#15655=DIRECTION('ref_axis',(0.224684645967589,0.974431531646231,-2.31111593326468E-33));
#15656=DIRECTION('',(0.974431531646231,-0.224684645967589,1.26428912495664E-17));
#15657=DIRECTION('center_axis',(-0.974431531646231,0.224684645967589,-1.26428912495664E-17));
#15658=DIRECTION('ref_axis',(0.224684645967589,0.974431531646231,-1.15555796663234E-33));
#15659=DIRECTION('center_axis',(-0.974431531646231,0.224684645967589,-1.26428912495664E-17));
#15660=DIRECTION('ref_axis',(0.224684645967589,0.974431531646231,-3.85185988877447E-34));
#15661=DIRECTION('center_axis',(-0.974431531646231,0.224684645967589,-1.26428912495664E-17));
#15662=DIRECTION('ref_axis',(0.224684645967589,0.974431531646231,-3.85185988877447E-34));
#15663=DIRECTION('',(0.974431531646231,-0.224684645967589,1.26428912495664E-17));
#15664=DIRECTION('center_axis',(-0.974431531646231,0.224684645967589,-1.26428912495664E-17));
#15665=DIRECTION('ref_axis',(0.224684645967589,0.974431531646231,-3.85185988877447E-34));
#15666=DIRECTION('center_axis',(-0.974431531646231,0.224684645967589,-1.26428912495664E-17));
#15667=DIRECTION('ref_axis',(0.224684645967589,0.974431531646231,-3.85185988877447E-34));
#15668=DIRECTION('center_axis',(-0.974431531646231,0.224684645967589,-1.26428912495664E-17));
#15669=DIRECTION('ref_axis',(0.224684645967589,0.974431531646231,-3.85185988877447E-34));
#15670=DIRECTION('center_axis',(-0.974431531646231,0.224684645967589,-1.26428912495664E-17));
#15671=DIRECTION('ref_axis',(0.224684645967589,0.974431531646231,-3.85185988877447E-34));
#15672=DIRECTION('center_axis',(-0.94183030799337,0.336088784319134,1.16739108769533E-16));
#15673=DIRECTION('ref_axis',(-0.336088784319135,-0.94183030799337,-6.36115566062716E-14));
#15674=DIRECTION('',(0.997691327175712,-0.0679118228172861,-6.86415162287128E-18));
#15675=DIRECTION('center_axis',(-0.974431531646231,0.224684645967589,-1.26428912495664E-17));
#15676=DIRECTION('ref_axis',(0.224684645967589,0.974431531646231,-2.31111593326468E-33));
#15677=DIRECTION('center_axis',(-0.974431531646231,0.224684645967589,-1.26428912495664E-17));
#15678=DIRECTION('ref_axis',(0.224684645967589,0.974431531646231,-2.31111593326468E-33));
#15679=DIRECTION('center_axis',(-0.974431531646231,0.224684645967589,-1.26428912495664E-17));
#15680=DIRECTION('ref_axis',(0.224684645967589,0.974431531646231,-2.31111593326468E-33));
#15681=DIRECTION('center_axis',(-0.974431531646231,0.224684645967589,-1.26428912495664E-17));
#15682=DIRECTION('ref_axis',(0.224684645967589,0.974431531646231,-2.31111593326468E-33));
#15683=DIRECTION('center_axis',(-0.974431531646231,0.224684645967589,-1.26428912495664E-17));
#15684=DIRECTION('ref_axis',(0.224684645967589,0.974431531646231,-2.31111593326468E-33));
#15685=DIRECTION('center_axis',(-2.08745462991212E-17,-1.24347063228184E-16,
1.));
#15686=DIRECTION('ref_axis',(0.974431531646231,-0.224684645967589,-7.59805975586113E-18));
#15687=DIRECTION('',(2.08745462991212E-17,1.24347063228184E-16,-1.));
#15688=DIRECTION('',(2.08745462991212E-17,1.24347063228184E-16,-1.));
#15689=DIRECTION('',(2.08745462991212E-17,1.24347063228184E-16,-1.));
#15690=DIRECTION('',(-2.08745462991212E-17,-1.24347063228184E-16,1.));
#15691=DIRECTION('center_axis',(-0.224684645967589,-0.974431531646231,-6.60780807231409E-17));
#15692=DIRECTION('ref_axis',(-0.974431531646231,0.224684645967589,-1.26428912495664E-17));
#15693=DIRECTION('',(-2.08745462991212E-17,-1.24347063228184E-16,1.));
#15694=DIRECTION('',(0.974431531646231,-0.224684645967589,1.26428912495664E-17));
#15695=DIRECTION('',(2.08745462991212E-17,1.24347063228184E-16,-1.));
#15696=DIRECTION('',(-0.974431531646231,0.224684645967589,-1.26428912495664E-17));
#15697=DIRECTION('center_axis',(2.08745462991212E-17,1.24347063228184E-16,
-1.));
#15698=DIRECTION('ref_axis',(-0.974431531646231,0.224684645967589,7.59805975586114E-18));
#15699=DIRECTION('',(2.08745462991212E-17,1.24347063228184E-16,-1.));
#15700=DIRECTION('center_axis',(0.224684645967589,0.974431531646231,6.60780807231409E-17));
#15701=DIRECTION('ref_axis',(0.974431531646231,-0.224684645967589,1.26428912495664E-17));
#15702=DIRECTION('',(2.08745462991212E-17,1.24347063228184E-16,-1.));
#15703=DIRECTION('',(0.974431531646231,-0.224684645967589,1.26428912495664E-17));
#15704=DIRECTION('',(-0.974431531646231,0.224684645967589,-1.26428912495664E-17));
#15705=DIRECTION('center_axis',(4.05979671893162E-17,1.19799232317482E-16,
-1.));
#15706=DIRECTION('ref_axis',(-0.974431531646231,0.224684645967589,-1.26428912495664E-17));
#15707=DIRECTION('center_axis',(4.05979671893162E-17,1.19799232317482E-16,
-1.));
#15708=DIRECTION('ref_axis',(-0.974431531646231,0.224684645967589,-1.26428912495664E-17));
#15709=DIRECTION('center_axis',(0.974431531646231,-0.224684645967589,1.26428912495664E-17));
#15710=DIRECTION('ref_axis',(-0.224684645967589,-0.974431531646231,-6.60780807231409E-17));
#15711=DIRECTION('center_axis',(-0.974431531646231,0.224684645967589,-1.26428912495664E-17));
#15712=DIRECTION('ref_axis',(-0.224684645967589,-0.974431531646231,-1.42518815884655E-32));
#15713=DIRECTION('center_axis',(-0.974431531646231,0.224684645967589,-1.26428912495664E-17));
#15714=DIRECTION('ref_axis',(-0.224684645967589,-0.974431531646231,-1.42518815884655E-32));
#15715=DIRECTION('center_axis',(0.974431531646231,-0.224684645967589,1.26428912495664E-17));
#15716=DIRECTION('ref_axis',(-0.224684645967589,-0.974431531646231,-6.60780807231409E-17));
#15717=DIRECTION('center_axis',(-0.974431531646231,0.224684645967589,-1.26428912495664E-17));
#15718=DIRECTION('ref_axis',(-0.224684645967589,-0.974431531646231,1.38777878078144E-14));
#15719=DIRECTION('center_axis',(-0.974431531646231,0.224684645967589,-1.26428912495664E-17));
#15720=DIRECTION('ref_axis',(-0.224684645967589,-0.974431531646231,-1.42518815884655E-32));
#15721=DIRECTION('center_axis',(-0.974431531646231,0.224684645967589,-1.26428912495664E-17));
#15722=DIRECTION('ref_axis',(0.224684645967589,0.974431531646231,6.60780807231409E-17));
#15723=DIRECTION('center_axis',(-0.974431531646231,0.224684645967589,-1.26428912495664E-17));
#15724=DIRECTION('ref_axis',(0.224684645967589,0.974431531646231,6.60780807231409E-17));
#15725=DIRECTION('center_axis',(-0.974431531646231,0.224684645967589,-1.26428912495664E-17));
#15726=DIRECTION('ref_axis',(0.224684645967589,0.974431531646231,6.60780807231409E-17));
#15727=DIRECTION('center_axis',(-0.974431531646231,0.224684645967589,-1.26428912495664E-17));
#15728=DIRECTION('ref_axis',(0.224684645967589,0.974431531646231,6.60780807231409E-17));
#15729=DIRECTION('',(0.112342322983794,0.487215765823115,-0.866025403784439));
#15730=DIRECTION('',(0.224684645967589,0.974431531646231,-9.52915449491201E-17));
#15731=DIRECTION('',(0.112342322983794,0.487215765823115,0.866025403784438));
#15732=DIRECTION('',(-0.112342322983794,-0.487215765823116,0.866025403784438));
#15733=DIRECTION('',(-0.224684645967589,-0.974431531646231,2.56661170621381E-16));
#15734=DIRECTION('',(-0.112342322983794,-0.487215765823116,-0.866025403784438));
#15735=DIRECTION('center_axis',(-0.194582611248245,-0.843882460654216,-0.5));
#15736=DIRECTION('ref_axis',(-0.112342322983794,-0.487215765823115,0.866025403784439));
#15737=DIRECTION('',(0.974431531646231,-0.224684645967589,1.26428912495664E-17));
#15738=DIRECTION('',(-0.112342322983794,-0.487215765823115,0.866025403784439));
#15739=DIRECTION('',(0.974431531646231,-0.224684645967589,1.26428912495664E-17));
#15740=DIRECTION('center_axis',(-0.194582611248245,-0.843882460654216,0.5));
#15741=DIRECTION('ref_axis',(0.112342322983794,0.487215765823116,0.866025403784438));
#15742=DIRECTION('',(0.974431531646231,-0.224684645967589,1.26428912495664E-17));
#15743=DIRECTION('',(0.112342322983794,0.487215765823116,0.866025403784438));
#15744=DIRECTION('center_axis',(6.50716132601352E-17,2.48391570236421E-16,
1.));
#15745=DIRECTION('ref_axis',(0.224684645967589,0.974431531646231,-2.56661170621381E-16));
#15746=DIRECTION('',(0.974431531646231,-0.224684645967589,1.26428912495664E-17));
#15747=DIRECTION('',(0.224684645967589,0.974431531646231,-2.56661170621381E-16));
#15748=DIRECTION('center_axis',(0.194582611248245,0.843882460654216,0.5));
#15749=DIRECTION('ref_axis',(0.112342322983794,0.487215765823116,-0.866025403784439));
#15750=DIRECTION('',(0.974431531646231,-0.224684645967589,1.26428912495664E-17));
#15751=DIRECTION('',(0.112342322983794,0.487215765823116,-0.866025403784438));
#15752=DIRECTION('center_axis',(0.194582611248245,0.843882460654216,-0.5));
#15753=DIRECTION('ref_axis',(-0.112342322983794,-0.487215765823116,-0.866025403784439));
#15754=DIRECTION('',(0.974431531646231,-0.224684645967589,1.26428912495664E-17));
#15755=DIRECTION('',(-0.112342322983794,-0.487215765823116,-0.866025403784438));
#15756=DIRECTION('center_axis',(-2.88143360460409E-17,-9.11479187314206E-17,
-1.));
#15757=DIRECTION('ref_axis',(-0.224684645967589,-0.974431531646231,9.52915449491202E-17));
#15758=DIRECTION('',(-0.224684645967589,-0.974431531646231,9.52915449491202E-17));
#15759=DIRECTION('center_axis',(-0.974431531646231,0.224684645967589,7.59805975586106E-18));
#15760=DIRECTION('ref_axis',(-2.08745462991212E-17,-1.24347063228184E-16,
1.));
#15761=DIRECTION('',(0.112342322983794,0.487215765823116,0.866025403784438));
#15762=DIRECTION('',(0.224684645967589,0.974431531646231,-9.52915449491202E-17));
#15763=DIRECTION('',(0.112342322983794,0.487215765823115,-0.866025403784439));
#15764=DIRECTION('',(-0.112342322983794,-0.487215765823116,-0.866025403784438));
#15765=DIRECTION('',(-0.224684645967589,-0.974431531646231,2.56661170621381E-16));
#15766=DIRECTION('',(-0.112342322983794,-0.487215765823116,0.866025403784438));
#15767=DIRECTION('center_axis',(0.224684645967589,0.974431531646231,1.25857889322102E-16));
#15768=DIRECTION('ref_axis',(2.08745462991212E-17,1.24347063228184E-16,
-1.));
#15769=DIRECTION('',(-0.974431531646231,0.224684645967589,1.09821788665169E-16));
#15770=DIRECTION('',(2.08745462991212E-17,1.24347063228184E-16,-1.));
#15771=DIRECTION('',(0.974431531646231,-0.224684645967589,1.26428912495664E-17));
#15772=DIRECTION('',(0.,0.,1.));
#15773=DIRECTION('',(0.974431531646231,-0.224684645967588,0.));
#15774=DIRECTION('',(-0.974431531646231,0.224684645967588,0.));
#15775=DIRECTION('',(0.,0.,1.));
#15776=DIRECTION('center_axis',(0.974431531646231,-0.224684645967589,-7.59805975586106E-18));
#15777=DIRECTION('ref_axis',(2.08745462991212E-17,1.24347063228184E-16,
-1.));
#15778=DIRECTION('',(0.224684645967589,0.974431531646231,6.60780807231409E-17));
#15779=DIRECTION('',(-0.224684645967589,-0.974431531646231,-6.60780807231409E-17));
#15780=DIRECTION('',(-2.08745462991212E-17,-1.24347063228184E-16,1.));
#15781=DIRECTION('',(-0.224684645967589,-0.974431531646231,-6.60780807231409E-17));
#15782=DIRECTION('',(0.224684645967589,0.974431531646231,6.60780807231409E-17));
#15783=DIRECTION('center_axis',(-1.08212737336466E-16,-1.04208603115422E-16,
1.));
#15784=DIRECTION('ref_axis',(0.974431531646231,-0.224684645967589,8.20318302886387E-17));
#15785=DIRECTION('',(0.336088784319134,0.94183030799337,9.58152703863411E-17));
#15786=DIRECTION('center_axis',(4.05979671893162E-17,1.19799232317482E-16,
-1.));
#15787=DIRECTION('ref_axis',(-0.974431531646231,0.224684645967589,-1.26428912495664E-17));
#15788=DIRECTION('',(0.336088784319134,0.94183030799337,6.70979889663902E-17));
#15789=DIRECTION('center_axis',(-0.94183030799337,0.336088784319134,1.16739108769533E-16));
#15790=DIRECTION('ref_axis',(0.336088784319134,0.94183030799337,6.70979889663902E-17));
#15791=DIRECTION('center_axis',(4.05979671893162E-17,1.19799232317482E-16,
-1.));
#15792=DIRECTION('ref_axis',(-0.974431531646231,0.224684645967589,-1.26428912495664E-17));
#15793=DIRECTION('',(-0.224684645967589,-0.974431531646231,-6.60780807231409E-17));
#15794=DIRECTION('center_axis',(-2.08745462991212E-17,-1.24347063228184E-16,
1.));
#15795=DIRECTION('ref_axis',(-0.974431531646231,0.224684645967587,7.59805975586085E-18));
#15796=DIRECTION('',(0.974431531646231,-0.224684645967589,1.26428912495664E-17));
#15797=DIRECTION('center_axis',(-0.974431531646231,0.224684645967589,7.59805975586106E-18));
#15798=DIRECTION('ref_axis',(-2.08745462991212E-17,-1.24347063228184E-16,
1.));
#15799=DIRECTION('',(-0.224684645967589,-0.974431531646231,-6.60780807231409E-17));
#15800=DIRECTION('',(-2.08745462991212E-17,-1.24347063228184E-16,1.));
#15801=DIRECTION('center_axis',(7.87354784325647E-17,-1.47315165567658E-16,
1.));
#15802=DIRECTION('ref_axis',(0.974431531646231,-0.224684645967589,-1.09821788665169E-16));
#15803=DIRECTION('',(-0.974431531646231,0.224684645967589,1.09821788665169E-16));
#15804=DIRECTION('center_axis',(-9.84588993227598E-17,1.5186299647836E-16,
-1.));
#15805=DIRECTION('ref_axis',(0.974431531646237,-0.224684645967561,-1.30062739670593E-16));
#15806=DIRECTION('center_axis',(-0.224684645967589,-0.974431531646231,-1.25857889322102E-16));
#15807=DIRECTION('ref_axis',(-2.08745462991212E-17,-1.24347063228184E-16,
1.));
#15808=DIRECTION('',(2.08745462991212E-17,1.24347063228184E-16,-1.));
#15809=DIRECTION('center_axis',(0.224684645967589,0.974431531646231,1.25857889322102E-16));
#15810=DIRECTION('ref_axis',(2.08745462991212E-17,1.24347063228184E-16,
-1.));
#15811=DIRECTION('',(-3.69499511157397E-16,2.14359602894637E-16,-1.));
#15812=DIRECTION('',(-0.843882460654216,0.194582611248245,-0.5));
#15813=DIRECTION('center_axis',(0.224684645967589,0.974431531646231,1.25857889322102E-16));
#15814=DIRECTION('ref_axis',(2.08745462991212E-17,1.24347063228184E-16,
-1.));
#15815=DIRECTION('',(-0.843882460654216,0.194582611248245,-0.5));
#15816=DIRECTION('',(-0.843882460654216,0.194582611248245,0.5));
#15817=DIRECTION('center_axis',(0.224684645967589,0.974431531646231,1.25857889322102E-16));
#15818=DIRECTION('ref_axis',(2.08745462991212E-17,1.24347063228184E-16,
-1.));
#15819=DIRECTION('',(-0.843882460654216,0.194582611248245,0.5));
#15820=DIRECTION('',(-1.18468060663251E-16,-1.01843928311571E-16,1.));
#15821=DIRECTION('center_axis',(0.224684645967589,0.974431531646231,1.25857889322102E-16));
#15822=DIRECTION('ref_axis',(2.08745462991212E-17,1.24347063228184E-16,
-1.));
#15823=DIRECTION('',(-1.18468060663251E-16,-1.01843928311571E-16,1.));
#15824=DIRECTION('',(0.843882460654216,-0.194582611248245,0.5));
#15825=DIRECTION('center_axis',(0.224684645967589,0.974431531646231,1.25857889322102E-16));
#15826=DIRECTION('ref_axis',(2.08745462991212E-17,1.24347063228184E-16,
-1.));
#15827=DIRECTION('',(0.843882460654216,-0.194582611248245,0.5));
#15828=DIRECTION('',(0.843882460654216,-0.194582611248245,-0.5));
#15829=DIRECTION('center_axis',(0.224684645967589,0.974431531646231,1.25857889322102E-16));
#15830=DIRECTION('ref_axis',(2.08745462991212E-17,1.24347063228184E-16,
-1.));
#15831=DIRECTION('',(0.843882460654216,-0.194582611248245,-0.5));
#15832=DIRECTION('',(-3.69499511157397E-16,2.14359602894637E-16,-1.));
#15833=DIRECTION('center_axis',(0.487215765823115,-0.112342322983794,-0.866025403784439));
#15834=DIRECTION('ref_axis',(-0.843882460654216,0.194582611248245,-0.5));
#15835=DIRECTION('',(-0.843882460654216,0.194582611248245,-0.5));
#15836=DIRECTION('center_axis',(-0.487215765823116,0.112342322983932,0.86602540378442));
#15837=DIRECTION('ref_axis',(-0.616523841583692,-0.746591155021291,-0.250000000005721));
#15838=DIRECTION('',(-0.224684645967589,-0.974431531646231,-6.60780807231409E-17));
#15839=DIRECTION('',(-0.224684645967589,-0.974431531646231,-6.60780807231409E-17));
#15840=DIRECTION('center_axis',(-0.487215765823115,0.112342322983794,-0.866025403784439));
#15841=DIRECTION('ref_axis',(-0.843882460654216,0.194582611248245,0.5));
#15842=DIRECTION('',(-0.843882460654216,0.194582611248245,0.5));
#15843=DIRECTION('',(-0.224684645967589,-0.974431531646231,-6.60780807231409E-17));
#15844=DIRECTION('center_axis',(0.487215765823073,-0.11234232298389,0.86602540378445));
#15845=DIRECTION('ref_axis',(0.227358619055838,-0.941173766287018,-0.249999999988262));
#15846=DIRECTION('center_axis',(-0.974431531646231,0.224684645967589,4.0821528608577E-16));
#15847=DIRECTION('ref_axis',(3.69499511157397E-16,-2.14359602894637E-16,
1.));
#15848=DIRECTION('',(3.69499511157397E-16,-2.14359602894637E-16,1.));
#15849=DIRECTION('center_axis',(0.974431531646239,-0.224684645967554,2.62889778835188E-14));
#15850=DIRECTION('ref_axis',(0.194582611247985,0.843882460653167,-0.500000000001871));
#15851=DIRECTION('',(-0.224684645967589,-0.974431531646231,-6.60780807231409E-17));
#15852=DIRECTION('center_axis',(0.974431531646148,-0.224684645967948,8.109997424295E-14));
#15853=DIRECTION('ref_axis',(0.194582611256729,0.843882460689772,0.499999999936689));
#15854=DIRECTION('center_axis',(-0.487215765823115,0.112342322983794,0.866025403784439));
#15855=DIRECTION('ref_axis',(0.843882460654216,-0.194582611248245,0.5));
#15856=DIRECTION('',(0.843882460654216,-0.194582611248245,0.5));
#15857=DIRECTION('center_axis',(0.487215765823131,-0.112342322983759,-0.866025403784434));
#15858=DIRECTION('ref_axis',(-0.22735861905635,0.941173766286857,-0.249999999988406));
#15859=DIRECTION('',(-0.224684645967589,-0.974431531646231,-6.60780807231409E-17));
#15860=DIRECTION('center_axis',(0.487215765823115,-0.112342322983794,0.866025403784439));
#15861=DIRECTION('ref_axis',(0.843882460654216,-0.194582611248245,-0.5));
#15862=DIRECTION('',(-0.224684645967589,-0.974431531646231,-6.60780807231409E-17));
#15863=DIRECTION('center_axis',(-0.487215765823103,0.112342322983935,-0.866025403784427));
#15864=DIRECTION('ref_axis',(0.616523841604247,0.746591154999503,-0.250000000020098));
#15865=DIRECTION('',(0.843882460654216,-0.194582611248245,-0.5));
#15866=DIRECTION('center_axis',(0.974431531646231,-0.224684645967589,9.25562468266162E-17));
#15867=DIRECTION('ref_axis',(1.18468060663251E-16,1.01843928311571E-16,
-1.));
#15868=DIRECTION('center_axis',(-0.974431531646193,0.224684645967751,2.94355350819261E-14));
#15869=DIRECTION('ref_axis',(0.194582611249943,0.843882460661004,-0.499999999987883));
#15870=DIRECTION('',(1.18468060663251E-16,1.01843928311571E-16,-1.));
#15871=DIRECTION('center_axis',(-0.974431531646256,0.224684645967479,3.31911033510058E-14));
#15872=DIRECTION('ref_axis',(0.194582611244197,0.843882460637021,0.500000000030596));
#15873=DIRECTION('center_axis',(0.224684645967589,0.974431531646231,1.25857889322102E-16));
#15874=DIRECTION('ref_axis',(2.08745462991212E-17,1.24347063228184E-16,
-1.));
#15875=DIRECTION('center_axis',(0.224684645967592,0.97443153164623,4.52473261763703E-15));
#15876=DIRECTION('ref_axis',(0.843882460654121,-0.194582611248228,0.500000000000167));
#15877=DIRECTION('center_axis',(0.22468464596757,0.974431531646235,1.02704248305103E-14));
#15878=DIRECTION('ref_axis',(0.843882460654164,-0.19458261124821,-0.500000000000101));
#15879=DIRECTION('center_axis',(0.224684645967572,0.974431531646235,-8.04396909802231E-15));
#15880=DIRECTION('ref_axis',(0.843882460654151,-0.194582611248211,0.500000000000123));
#15881=DIRECTION('center_axis',(0.224684645967561,0.974431531646237,1.49387997534668E-14));
#15882=DIRECTION('ref_axis',(0.843882460654115,-0.194582611248188,-0.500000000000192));
#15883=DIRECTION('center_axis',(-0.185637535122341,0.768465162225134,0.612372435695795));
#15884=DIRECTION('ref_axis',(-0.843882460654216,0.194582611248245,-0.5));
#15885=DIRECTION('',(-0.785005807280206,-0.490824550811397,0.377964473009226));
#15886=DIRECTION('center_axis',(0.503389608706702,0.609589125432954,0.612372435695794));
#15887=DIRECTION('ref_axis',(-0.843882460654216,0.194582611248245,0.5));
#15888=DIRECTION('',(-0.490824550811399,0.785005807280205,-0.377964473009226));
#15889=DIRECTION('center_axis',(-0.530151107036863,0.847903180621225,2.35478172332082E-17));
#15890=DIRECTION('ref_axis',(1.18468060663251E-16,1.01843928311571E-16,
-1.));
#15891=DIRECTION('',(0.785005807280206,0.490824550811397,-0.377964473009226));
#15892=DIRECTION('',(-0.785005807280206,-0.490824550811397,-0.377964473009227));
#15893=DIRECTION('center_axis',(0.847903180621223,0.530151107036865,-1.99656829969769E-16));
#15894=DIRECTION('ref_axis',(3.69499511157397E-16,-2.14359602894637E-16,
1.));
#15895=DIRECTION('',(-0.4908245508114,0.785005807280206,0.377964473009223));
#15896=DIRECTION('',(0.490824550811399,-0.785005807280205,0.377964473009226));
#15897=DIRECTION('center_axis',(-0.185637535122341,0.768465162225134,-0.612372435695794));
#15898=DIRECTION('ref_axis',(0.843882460654216,-0.194582611248245,-0.5));
#15899=DIRECTION('',(0.785005807280206,0.490824550811397,0.377964473009226));
#15900=DIRECTION('center_axis',(0.503389608706703,0.609589125432952,-0.612372435695796));
#15901=DIRECTION('ref_axis',(0.843882460654216,-0.194582611248245,0.5));
#15902=DIRECTION('',(0.4908245508114,-0.785005807280206,-0.377964473009223));
#15903=DIRECTION('center_axis',(0.4908245508114,-0.785005807280206,-0.377964473009223));
#15904=DIRECTION('ref_axis',(-0.847903180621223,-0.530151107036865,-2.77555756156289E-17));
#15905=DIRECTION('center_axis',(9.16975147669649E-9,5.73796578879224E-9,
1.));
#15906=DIRECTION('ref_axis',(0.530161597891661,-0.847896621128402,3.75170931248065E-12));
#15907=DIRECTION('center_axis',(0.490824550811399,-0.785005807280205,0.377964473009226));
#15908=DIRECTION('ref_axis',(-0.847903180621223,-0.530151107036865,5.55111512312578E-17));
#15909=DIRECTION('center_axis',(0.785005807280206,0.490824550811397,0.377964473009227));
#15910=DIRECTION('ref_axis',(0.530151107036863,-0.847903180621225,-2.77555756156289E-16));
#15911=DIRECTION('center_axis',(-2.08293517271166E-9,3.33669624293654E-9,
1.));
#15912=DIRECTION('ref_axis',(0.847906432817937,0.530145905563706,-2.8017192176462E-12));
#15913=DIRECTION('center_axis',(0.785005807280206,0.490824550811397,-0.377964473009226));
#15914=DIRECTION('ref_axis',(0.530151107036863,-0.847903180621224,3.05311331771918E-16));
#15915=DIRECTION('center_axis',(-0.974431531646231,0.224684645967589,-1.26428912495664E-17));
#15916=DIRECTION('ref_axis',(0.224684645967589,0.974431531646231,1.23259516440783E-32));
#15917=DIRECTION('',(-0.974431531646231,0.224684645967589,-1.26428912495664E-17));
#15918=DIRECTION('',(0.974431531646231,-0.224684645967589,1.26428912495664E-17));
#15919=DIRECTION('center_axis',(-0.974431531646231,0.224684645967589,-1.26428912495664E-17));
#15920=DIRECTION('ref_axis',(0.224684645967589,0.974431531646231,1.23259516440783E-32));
#15921=DIRECTION('',(0.974431531646231,-0.224684645967589,1.26428912495664E-17));
#15922=DIRECTION('',(-0.974431531646231,0.224684645967589,-1.26428912495664E-17));
#15923=DIRECTION('center_axis',(0.224684645967589,0.974431531646231,1.25857889322102E-16));
#15924=DIRECTION('ref_axis',(2.08745462991212E-17,1.24347063228184E-16,
-1.));
#15925=DIRECTION('center_axis',(-0.974431531646231,0.224684645967589,7.59805975586106E-18));
#15926=DIRECTION('ref_axis',(-2.08745462991212E-17,-1.24347063228184E-16,
1.));
#15927=DIRECTION('center_axis',(-0.974431531646231,0.224684645967589,-1.26428912495664E-17));
#15928=DIRECTION('ref_axis',(0.224684645967589,0.974431531646231,1.42518815884655E-32));
#15929=DIRECTION('center_axis',(0.974431531646231,-0.224684645967589,1.26428912495664E-17));
#15930=DIRECTION('ref_axis',(1.23196318847518E-17,-2.84066354441556E-18,
-1.));
#15931=DIRECTION('center_axis',(0.0216454139389726,-0.98876345800245,-0.147913150782639));
#15932=DIRECTION('ref_axis',(-0.999760469446545,-0.021886153888323,1.85181731060524E-16));
#15933=DIRECTION('center_axis',(-0.843042330772965,-0.426528196188075,0.327648174695716));
#15934=DIRECTION('ref_axis',(-0.451448225784322,0.892297315605168,-2.31759056390501E-15));
#15935=DIRECTION('center_axis',(-0.974431531646231,0.224684645967589,-1.26428912495664E-17));
#15936=DIRECTION('ref_axis',(0.224684645967589,0.974431531646231,1.42518815884655E-32));
#15937=DIRECTION('center_axis',(-2.08745462991212E-17,-1.24347063228184E-16,
1.));
#15938=DIRECTION('ref_axis',(-0.974431531646231,0.224684645967589,7.59805975586112E-18));
#15939=DIRECTION('center_axis',(-0.974431531646231,0.224684645967589,-1.26428912495664E-17));
#15940=DIRECTION('ref_axis',(0.224684645967589,0.974431531646231,1.42518815884655E-32));
#15941=DIRECTION('center_axis',(0.974431531646231,-0.224684645967589,1.26428912495664E-17));
#15942=DIRECTION('ref_axis',(1.23196318847518E-17,-2.84066354441556E-18,
-1.));
#15943=DIRECTION('center_axis',(-2.08745462991212E-17,-1.24347063228184E-16,
1.));
#15944=DIRECTION('ref_axis',(0.974431531646231,-0.224684645967589,-7.59805975586112E-18));
#15945=DIRECTION('center_axis',(-2.08745462991212E-17,-1.24347063228184E-16,
1.));
#15946=DIRECTION('ref_axis',(0.974431531646231,-0.224684645967589,-7.59805975586112E-18));
#15947=DIRECTION('center_axis',(-0.974431531646231,0.224684645967589,-1.26428912495664E-17));
#15948=DIRECTION('ref_axis',(0.224684645967589,0.974431531646231,1.42518815884655E-32));
#15949=DIRECTION('center_axis',(0.843042330772967,0.426528196188067,0.327648174695721));
#15950=DIRECTION('ref_axis',(-0.451448225784312,0.892297315605173,-3.66373598126302E-15));
#15951=DIRECTION('center_axis',(0.021645413938973,-0.98876345800245,0.14791315078264));
#15952=DIRECTION('ref_axis',(-0.999760469446545,-0.0218861538883235,-1.16226472890446E-16));
#15953=DIRECTION('center_axis',(0.224684645967589,0.974431531646231,-2.56661170621381E-16));
#15954=DIRECTION('ref_axis',(-5.76678242546919E-17,-2.50098737602707E-16,
-1.));
#15955=DIRECTION('center_axis',(0.19458261124829,0.843882460654178,0.500000000000046));
#15956=DIRECTION('ref_axis',(-0.112342322997118,-0.48721576582009,0.866025403784412));
#15957=DIRECTION('center_axis',(-0.19458261124826,-0.843882460654214,0.499999999999998));
#15958=DIRECTION('ref_axis',(-0.11234232298209,-0.487215765823506,-0.86602540378444));
#15959=DIRECTION('center_axis',(0.112342322983794,0.487215765823116,-0.866025403784439));
#15960=DIRECTION('ref_axis',(-0.194582611248246,-0.843882460654216,-0.5));
#15961=DIRECTION('center_axis',(0.,0.,1.));
#15962=DIRECTION('ref_axis',(-0.224684645969392,-0.974431531645815,0.));
#15963=DIRECTION('center_axis',(0.112342322983794,0.487215765823116,0.866025403784439));
#15964=DIRECTION('ref_axis',(0.194582611248243,0.843882460654216,-0.5));
#15965=DIRECTION('center_axis',(0.,0.,1.));
#15966=DIRECTION('ref_axis',(-0.224684645964876,-0.974431531646856,0.));
#15967=DIRECTION('center_axis',(-0.112342322983794,-0.487215765823116,-0.866025403784439));
#15968=DIRECTION('ref_axis',(-0.194582611248246,-0.843882460654216,0.5));
#15969=DIRECTION('center_axis',(0.194582611248052,0.843882460654175,0.500000000000144));
#15970=DIRECTION('ref_axis',(-0.112342322985073,-0.487215765822968,0.866025403784356));
#15971=DIRECTION('center_axis',(-0.112342322983794,-0.487215765823115,0.866025403784439));
#15972=DIRECTION('ref_axis',(0.194582611248243,0.843882460654217,0.5));
#15973=DIRECTION('center_axis',(-0.19458261124824,-0.843882460654216,0.500000000000002));
#15974=DIRECTION('ref_axis',(-0.112342322980795,-0.487215765823809,-0.866025403784437));
#15975=DIRECTION('center_axis',(-0.224684645967589,-0.974431531646231,9.52915449491202E-17));
#15976=DIRECTION('ref_axis',(2.14105470405976E-17,9.28550860977068E-17,
1.));
#15977=DIRECTION('center_axis',(2.08745462991212E-17,1.24347063228184E-16,
-1.));
#15978=DIRECTION('ref_axis',(-0.974431531646231,0.224684645967587,7.59805975586085E-18));
#15979=DIRECTION('axis',(0.,0.,1.));
#15980=DIRECTION('refdir',(1.,0.,0.));
#15981=DIRECTION('center_axis',(0.974431531646231,-0.224684645967589,-3.15685775282419E-17));
#15982=DIRECTION('ref_axis',(-0.224684645967589,-0.974431531646231,7.70371977754894E-33));
#15983=DIRECTION('center_axis',(0.974431531646231,-0.224684645967589,-3.15685775282419E-17));
#15984=DIRECTION('ref_axis',(0.224684645967589,0.974431531646231,-7.70371977754894E-33));
#15985=DIRECTION('center_axis',(0.974431531646231,-0.224684645967589,-3.15685775282419E-17));
#15986=DIRECTION('ref_axis',(0.224684645967589,0.974431531646231,3.96508223080413E-15));
#15987=DIRECTION('',(-0.847903180621224,-0.530151107036863,-6.42732503809162E-17));
#15988=DIRECTION('center_axis',(-0.974431531646231,0.224684645967589,3.15685775282419E-17));
#15989=DIRECTION('ref_axis',(0.224684645967589,0.974431531646231,1.00148357108136E-32));
#15990=DIRECTION('center_axis',(0.974431531646231,-0.224684645967589,-3.15685775282419E-17));
#15991=DIRECTION('ref_axis',(0.224684645967589,0.974431531646231,3.96508223080413E-15));
#15992=DIRECTION('center_axis',(1.41649888995139E-16,-4.54281045584161E-17,
1.));
#15993=DIRECTION('ref_axis',(-0.974431531646231,0.224684645967588,1.48235115880738E-16));
#15994=DIRECTION('',(-1.41649888995139E-16,4.54281045584162E-17,-1.));
#15995=DIRECTION('center_axis',(-1.41649888995139E-16,4.54281045584161E-17,
-1.));
#15996=DIRECTION('ref_axis',(0.974431531646231,-0.224684645967588,-1.48235115880738E-16));
#15997=DIRECTION('center_axis',(1.41649888995139E-16,-4.54281045584161E-17,
1.));
#15998=DIRECTION('ref_axis',(-0.974431531646231,0.224684645967588,1.48235115880738E-16));
#15999=DIRECTION('center_axis',(-1.41649888995139E-16,4.54281045584161E-17,
-1.));
#16000=DIRECTION('ref_axis',(0.974431531646231,-0.224684645967588,-1.48235115880738E-16));
#16001=DIRECTION('',(-1.41649888995139E-16,4.54281045584162E-17,-1.));
#16002=DIRECTION('center_axis',(-0.974431531646231,0.224684645967589,3.15685775282419E-17));
#16003=DIRECTION('ref_axis',(0.224684645967589,0.974431531646231,1.00148357108136E-32));
#16004=DIRECTION('center_axis',(0.974431531646231,-0.224684645967589,-3.15685775282419E-17));
#16005=DIRECTION('ref_axis',(-0.224684645967589,-0.974431531646231,7.70371977754894E-33));
#16006=DIRECTION('',(0.612348034572362,0.790588315468528,-1.24422025962473E-16));
#16007=DIRECTION('center_axis',(-0.974431531646231,0.224684645967589,3.15685775282419E-17));
#16008=DIRECTION('ref_axis',(-3.07614173527375E-17,7.09297466563341E-18,
-1.));
#16009=DIRECTION('center_axis',(-0.974431531646231,0.224684645967589,3.15685775282419E-17));
#16010=DIRECTION('ref_axis',(-3.07614173527375E-17,7.09297466563341E-18,
-1.));
#16011=DIRECTION('center_axis',(0.974431531646231,-0.224684645967589,-3.15685775282419E-17));
#16012=DIRECTION('ref_axis',(-0.224684645967589,-0.974431531646231,7.70371977754894E-33));
#16013=DIRECTION('center_axis',(0.974431531646231,-0.224684645967589,-3.15685775282419E-17));
#16014=DIRECTION('ref_axis',(3.07614173527375E-17,-7.09297466563341E-18,
1.));
#16015=DIRECTION('center_axis',(-0.974431531646231,0.224684645967589,3.15685775282419E-17));
#16016=DIRECTION('ref_axis',(-3.07614173527375E-17,7.09297466563341E-18,
-1.));
#16017=DIRECTION('',(-0.974431531646231,0.224684645967589,3.15685775282419E-17));
#16018=DIRECTION('center_axis',(0.974431531646231,-0.224684645967589,-3.15685775282419E-17));
#16019=DIRECTION('ref_axis',(-0.224684645967589,-0.974431531646231,7.70371977754894E-33));
#16020=DIRECTION('',(-0.974431531646231,0.224684645967589,3.15685775282419E-17));
#16021=DIRECTION('center_axis',(-0.974431531646231,0.224684645967589,1.48235115880738E-16));
#16022=DIRECTION('ref_axis',(-1.41649888995139E-16,4.54281045584161E-17,
-1.));
#16023=DIRECTION('center_axis',(-0.974431531646231,0.224684645967589,3.15685775282419E-17));
#16024=DIRECTION('ref_axis',(0.224684645967589,0.974431531646231,3.23381123402325E-17));
#16025=DIRECTION('center_axis',(-2.79663353364523E-17,1.92149246924214E-17,
-1.));
#16026=DIRECTION('ref_axis',(0.974431531646231,-0.224684645967589,-3.15685775282419E-17));
#16027=DIRECTION('center_axis',(-2.79663353364523E-17,1.92149246924214E-17,
-1.));
#16028=DIRECTION('ref_axis',(0.974431531646231,-0.224684645967589,-3.15685775282419E-17));
#16029=DIRECTION('axis',(0.,0.,1.));
#16030=DIRECTION('refdir',(1.,0.,0.));
#16031=DIRECTION('center_axis',(0.224684645967588,0.974431531646231,6.6078080723141E-17));
#16032=DIRECTION('ref_axis',(0.893873580715705,-0.206109575173111,0.398131717802593));
#16033=DIRECTION('center_axis',(0.224684645967588,0.974431531646231,6.6078080723141E-17));
#16034=DIRECTION('ref_axis',(0.893873580715705,-0.206109575173111,0.398131717802593));
#16035=DIRECTION('',(-0.224684645967588,-0.974431531646231,-6.6078080723141E-17));
#16036=DIRECTION('center_axis',(0.224684645967588,0.974431531646231,6.6078080723141E-17));
#16037=DIRECTION('ref_axis',(0.893873580715705,-0.206109575173111,0.398131717802593));
#16038=DIRECTION('center_axis',(0.224684645967588,0.974431531646231,6.6078080723141E-17));
#16039=DIRECTION('ref_axis',(0.893873580715709,-0.206109575173112,0.398131717802583));
#16040=DIRECTION('center_axis',(0.224684645967588,0.974431531646231,6.6078080723141E-17));
#16041=DIRECTION('ref_axis',(0.893873580715709,-0.206109575173112,0.398131717802583));
#16042=DIRECTION('',(-0.224684645967588,-0.974431531646231,-6.6078080723141E-17));
#16043=DIRECTION('center_axis',(0.224684645967588,0.974431531646231,6.6078080723141E-17));
#16044=DIRECTION('ref_axis',(0.893873580715709,-0.206109575173112,0.398131717802583));
#16045=DIRECTION('center_axis',(0.224684645967588,0.974431531646231,6.6078080723141E-17));
#16046=DIRECTION('ref_axis',(0.893873580715707,-0.206109575173112,0.398131717802588));
#16047=DIRECTION('center_axis',(0.224684645967588,0.974431531646231,6.6078080723141E-17));
#16048=DIRECTION('ref_axis',(0.893873580715705,-0.206109575173111,0.398131717802593));
#16049=DIRECTION('',(-0.224684645967588,-0.974431531646231,-6.6078080723141E-17));
#16050=DIRECTION('center_axis',(0.224684645967588,0.974431531646231,6.6078080723141E-17));
#16051=DIRECTION('ref_axis',(0.893873580715707,-0.206109575173112,0.398131717802588));
#16052=DIRECTION('center_axis',(0.224684645967588,0.974431531646231,6.6078080723141E-17));
#16053=DIRECTION('ref_axis',(0.893873580715709,-0.206109575173112,0.398131717802583));
#16054=DIRECTION('center_axis',(0.224684645967588,0.974431531646231,6.6078080723141E-17));
#16055=DIRECTION('ref_axis',(0.893873580715709,-0.206109575173112,0.398131717802583));
#16056=DIRECTION('',(-0.224684645967588,-0.974431531646231,-6.6078080723141E-17));
#16057=DIRECTION('center_axis',(0.224684645967588,0.974431531646231,6.6078080723141E-17));
#16058=DIRECTION('ref_axis',(0.893873580715709,-0.206109575173112,0.398131717802583));
#16059=DIRECTION('center_axis',(0.224684645967588,0.974431531646231,6.6078080723141E-17));
#16060=DIRECTION('ref_axis',(0.893873580715707,-0.206109575173112,0.398131717802588));
#16061=DIRECTION('center_axis',(0.224684645967588,0.974431531646231,6.6078080723141E-17));
#16062=DIRECTION('ref_axis',(0.893873580715707,-0.206109575173112,0.398131717802588));
#16063=DIRECTION('',(-0.224684645967588,-0.974431531646231,-6.6078080723141E-17));
#16064=DIRECTION('center_axis',(0.224684645967588,0.974431531646231,6.6078080723141E-17));
#16065=DIRECTION('ref_axis',(0.893873580715707,-0.206109575173112,0.398131717802588));
#16066=DIRECTION('center_axis',(-0.224684645967588,-0.974431531646231,-2.77555756156289E-17));
#16067=DIRECTION('ref_axis',(-0.893873580715708,0.206109575173112,-0.398131717802585));
#16068=DIRECTION('center_axis',(0.224684645967588,0.974431531646231,2.77555756156289E-17));
#16069=DIRECTION('ref_axis',(0.893873580715708,-0.206109575173112,0.398131717802585));
#16070=DIRECTION('center_axis',(-0.224684645967588,-0.974431531646231,-2.77555756156289E-17));
#16071=DIRECTION('ref_axis',(-0.893873580715708,0.206109575173112,-0.398131717802585));
#16072=DIRECTION('center_axis',(0.224684645967588,0.974431531646231,2.77555756156289E-17));
#16073=DIRECTION('ref_axis',(0.893873580715708,-0.206109575173112,0.398131717802585));
#16074=DIRECTION('center_axis',(-0.224684645967588,-0.974431531646231,-2.77555756156289E-17));
#16075=DIRECTION('ref_axis',(-0.893873580715708,0.206109575173112,-0.398131717802585));
#16076=DIRECTION('center_axis',(0.224684645967588,0.974431531646231,2.77555756156289E-17));
#16077=DIRECTION('ref_axis',(0.893873580715708,-0.206109575173112,0.398131717802585));
#16078=DIRECTION('axis',(0.,0.,1.));
#16079=DIRECTION('refdir',(1.,0.,0.));
#16080=DIRECTION('center_axis',(-0.224684645967588,-0.974431531646231,-6.6078080723141E-17));
#16081=DIRECTION('ref_axis',(-0.893873580715706,0.206109575173111,-0.398131717802591));
#16082=DIRECTION('center_axis',(-0.38795209957532,0.0894540840629421,0.917328259283208));
#16083=DIRECTION('ref_axis',(0.893873580715707,-0.206109575173114,0.398131717802587));
#16084=DIRECTION('center_axis',(0.224684645967588,0.974431531646231,6.6078080723141E-17));
#16085=DIRECTION('ref_axis',(-0.893873580715706,0.206109575173111,-0.39813171780259));
#16086=DIRECTION('axis',(0.,0.,1.));
#16087=DIRECTION('refdir',(1.,0.,0.));
#16088=DIRECTION('center_axis',(0.224684645967588,0.974431531646231,6.6078080723141E-17));
#16089=DIRECTION('ref_axis',(-2.99720887206891E-16,1.29778303242548E-18,
1.));
#16090=DIRECTION('',(-2.99720887206891E-16,1.29778303242547E-18,1.));
#16091=DIRECTION('',(0.689027143829045,-0.158876036792181,-0.707106781186546));
#16092=DIRECTION('',(0.974431531646231,-0.224684645967588,2.92349075108561E-16));
#16093=DIRECTION('',(2.99720887206891E-16,-1.29778303242547E-18,-1.));
#16094=DIRECTION('',(0.974431531646231,-0.224684645967588,2.92349075108561E-16));
#16095=DIRECTION('',(-0.689027143829042,0.15887603679218,-0.707106781186549));
#16096=DIRECTION('',(-2.99720887206891E-16,1.29778303242547E-18,1.));
#16097=DIRECTION('center_axis',(-0.224684645967588,-0.974431531646231,-6.6078080723141E-17));
#16098=DIRECTION('ref_axis',(1.48467301734967E-17,6.43885654072936E-17,
-1.));
#16099=DIRECTION('center_axis',(0.224684645967588,0.974431531646231,6.6078080723141E-17));
#16100=DIRECTION('ref_axis',(-2.99720887206891E-16,1.29778303242548E-18,
1.));
#16101=DIRECTION('',(0.974431531646231,-0.224684645967588,2.92349075108561E-16));
#16102=DIRECTION('',(-0.689027143829045,0.158876036792181,0.707106781186546));
#16103=DIRECTION('',(2.99720887206891E-16,-1.29778303242547E-18,-1.));
#16104=DIRECTION('center_axis',(0.224684645967588,0.974431531646231,6.6078080723141E-17));
#16105=DIRECTION('ref_axis',(-1.48467301734967E-17,-6.43885654072936E-17,
1.));
#16106=DIRECTION('',(2.99720887206891E-16,-1.29778303242547E-18,-1.));
#16107=DIRECTION('',(0.689027143829042,-0.15887603679218,0.707106781186549));
#16108=DIRECTION('',(0.974431531646231,-0.224684645967588,2.92349075108561E-16));
#16109=DIRECTION('',(2.99720887206891E-16,-1.29778303242547E-18,-1.));
#16110=DIRECTION('center_axis',(-2.99720887206891E-16,1.29778303242549E-18,
1.));
#16111=DIRECTION('ref_axis',(0.974431531646231,-0.224684645967588,2.92349075108561E-16));
#16112=DIRECTION('',(-0.224684645967588,-0.974431531646231,-6.60780807231409E-17));
#16113=DIRECTION('center_axis',(-2.99720887206891E-16,1.29778303242547E-18,
1.));
#16114=DIRECTION('ref_axis',(0.974431531646231,-0.224684645967589,2.92349075108561E-16));
#16115=DIRECTION('',(0.224684645967588,0.974431531646231,6.60780807231409E-17));
#16116=DIRECTION('center_axis',(-2.99720887206891E-16,1.29778303242547E-18,
1.));
#16117=DIRECTION('ref_axis',(0.974431531646231,-0.224684645967587,2.92349075108561E-16));
#16118=DIRECTION('',(-0.974431531646231,0.224684645967588,-2.92349075108561E-16));
#16119=DIRECTION('center_axis',(-2.99720887206891E-16,1.29778303242547E-18,
1.));
#16120=DIRECTION('ref_axis',(0.974431531646231,-0.224684645967587,2.92349075108561E-16));
#16121=DIRECTION('',(-0.224684645967588,-0.974431531646231,-6.60780807231409E-17));
#16122=DIRECTION('center_axis',(-2.99720887206891E-16,1.29778303242547E-18,
1.));
#16123=DIRECTION('ref_axis',(0.974431531646231,-0.224684645967589,2.92349075108561E-16));
#16124=DIRECTION('',(0.974431531646231,-0.224684645967588,2.92349075108561E-16));
#16125=DIRECTION('',(0.224684645967588,0.974431531646231,6.60780807231409E-17));
#16126=DIRECTION('',(0.974431531646231,-0.224684645967588,2.92349075108561E-16));
#16127=DIRECTION('center_axis',(-2.99720887206891E-16,1.29778303242547E-18,
1.));
#16128=DIRECTION('ref_axis',(-0.974431531646231,0.224684645967589,-2.92349075108561E-16));
#16129=DIRECTION('',(-0.224684645967588,-0.974431531646231,-6.60780807231409E-17));
#16130=DIRECTION('center_axis',(-2.99720887206891E-16,1.29778303242547E-18,
1.));
#16131=DIRECTION('ref_axis',(-0.974431531646231,0.224684645967589,-2.92349075108561E-16));
#16132=DIRECTION('',(-0.974431531646231,0.224684645967588,-2.92349075108561E-16));
#16133=DIRECTION('center_axis',(-2.99720887206891E-16,1.29778303242547E-18,
1.));
#16134=DIRECTION('ref_axis',(-0.974431531646231,0.224684645967589,-2.92349075108561E-16));
#16135=DIRECTION('',(0.224684645967588,0.974431531646231,6.60780807231409E-17));
#16136=DIRECTION('center_axis',(-2.99720887206891E-16,1.29778303242547E-18,
1.));
#16137=DIRECTION('ref_axis',(0.974431531646231,-0.224684645967589,2.92349075108561E-16));
#16138=DIRECTION('center_axis',(-2.99720887206891E-16,1.29778303242549E-18,
1.));
#16139=DIRECTION('ref_axis',(0.974431531646231,-0.224684645967588,2.92349075108561E-16));
#16140=DIRECTION('',(0.974431531646231,-0.224684645967588,2.92349075108561E-16));
#16141=DIRECTION('',(-0.224684645967588,-0.974431531646231,-6.60780807231409E-17));
#16142=DIRECTION('',(0.974431531646231,-0.224684645967588,2.92349075108561E-16));
#16143=DIRECTION('center_axis',(-2.99720887206891E-16,1.29778303242547E-18,
1.));
#16144=DIRECTION('ref_axis',(0.974431531646231,-0.224684645967589,2.92349075108561E-16));
#16145=DIRECTION('',(-0.224684645967588,-0.974431531646231,-6.60780807231409E-17));
#16146=DIRECTION('center_axis',(-2.99720887206891E-16,1.29778303242547E-18,
1.));
#16147=DIRECTION('ref_axis',(0.974431531646231,-0.224684645967587,2.92349075108561E-16));
#16148=DIRECTION('',(-0.974431531646231,0.224684645967588,-2.92349075108561E-16));
#16149=DIRECTION('center_axis',(-2.99720887206891E-16,1.29778303242547E-18,
1.));
#16150=DIRECTION('ref_axis',(0.974431531646231,-0.224684645967587,2.92349075108561E-16));
#16151=DIRECTION('',(0.224684645967588,0.974431531646231,6.60780807231409E-17));
#16152=DIRECTION('center_axis',(-2.99720887206891E-16,1.29778303242547E-18,
1.));
#16153=DIRECTION('ref_axis',(0.974431531646231,-0.224684645967589,2.92349075108561E-16));
#16154=DIRECTION('',(0.224684645967588,0.974431531646231,6.60780807231409E-17));
#16155=DIRECTION('center_axis',(-2.99720887206891E-16,1.29778303242547E-18,
1.));
#16156=DIRECTION('ref_axis',(0.974431531646231,-0.224684645967589,2.92349075108561E-16));
#16157=DIRECTION('',(0.224684645967588,0.974431531646231,6.60780807231409E-17));
#16158=DIRECTION('center_axis',(-2.99720887206891E-16,1.29778303242547E-18,
1.));
#16159=DIRECTION('ref_axis',(-0.974431531646231,0.224684645967589,-2.92349075108561E-16));
#16160=DIRECTION('',(-0.974431531646231,0.224684645967588,-2.92349075108561E-16));
#16161=DIRECTION('center_axis',(-2.99720887206891E-16,1.29778303242547E-18,
1.));
#16162=DIRECTION('ref_axis',(-0.974431531646231,0.224684645967589,-2.92349075108561E-16));
#16163=DIRECTION('',(-0.224684645967588,-0.974431531646231,-6.60780807231409E-17));
#16164=DIRECTION('center_axis',(-2.99720887206891E-16,1.29778303242547E-18,
1.));
#16165=DIRECTION('ref_axis',(-0.974431531646231,0.224684645967589,-2.92349075108561E-16));
#16166=DIRECTION('center_axis',(2.99720887206891E-16,-1.29778303242547E-18,
-1.));
#16167=DIRECTION('ref_axis',(-0.974431531646231,0.224684645967589,-2.92349075108561E-16));
#16168=DIRECTION('',(2.99720887206891E-16,-1.29778303242547E-18,-1.));
#16169=DIRECTION('center_axis',(-0.974431531646231,0.224684645967588,-2.92349075108561E-16));
#16170=DIRECTION('ref_axis',(-2.99720887206891E-16,1.29778303242548E-18,
1.));
#16171=DIRECTION('',(2.99720887206891E-16,-1.29778303242547E-18,-1.));
#16172=DIRECTION('center_axis',(2.99720887206891E-16,-1.29778303242547E-18,
-1.));
#16173=DIRECTION('ref_axis',(-0.974431531646231,0.224684645967587,-2.92349075108561E-16));
#16174=DIRECTION('',(2.99720887206891E-16,-1.29778303242547E-18,-1.));
#16175=DIRECTION('center_axis',(-0.224684645967588,-0.974431531646231,-6.6078080723141E-17));
#16176=DIRECTION('ref_axis',(2.99720887206891E-16,-1.29778303242548E-18,
-1.));
#16177=DIRECTION('',(2.99720887206891E-16,-1.29778303242547E-18,-1.));
#16178=DIRECTION('center_axis',(2.99720887206891E-16,-1.29778303242547E-18,
-1.));
#16179=DIRECTION('ref_axis',(-0.974431531646231,0.224684645967587,-2.92349075108561E-16));
#16180=DIRECTION('',(2.99720887206891E-16,-1.29778303242547E-18,-1.));
#16181=DIRECTION('center_axis',(0.974431531646231,-0.224684645967588,2.92349075108561E-16));
#16182=DIRECTION('ref_axis',(2.99720887206891E-16,-1.29778303242548E-18,
-1.));
#16183=DIRECTION('',(2.99720887206891E-16,-1.29778303242547E-18,-1.));
#16184=DIRECTION('center_axis',(2.99720887206891E-16,-1.29778303242547E-18,
-1.));
#16185=DIRECTION('ref_axis',(-0.974431531646231,0.224684645967589,-2.92349075108561E-16));
#16186=DIRECTION('',(2.99720887206891E-16,-1.29778303242547E-18,-1.));
#16187=DIRECTION('center_axis',(0.224684645967588,0.974431531646231,6.6078080723141E-17));
#16188=DIRECTION('ref_axis',(-2.99720887206891E-16,1.29778303242548E-18,
1.));
#16189=DIRECTION('',(0.689027143829042,-0.15887603679218,0.707106781186549));
#16190=DIRECTION('',(2.99720887206891E-16,-1.29778303242547E-18,-1.));
#16191=DIRECTION('center_axis',(-0.224684645967588,-0.974431531646231,-6.6078080723141E-17));
#16192=DIRECTION('ref_axis',(1.48467301734967E-17,6.43885654072936E-17,
-1.));
#16193=DIRECTION('',(2.99720887206891E-16,-1.29778303242547E-18,-1.));
#16194=DIRECTION('',(-0.689027143829045,0.158876036792181,0.707106781186546));
#16195=DIRECTION('center_axis',(2.99720887206891E-16,-1.29778303242547E-18,
-1.));
#16196=DIRECTION('ref_axis',(-0.974431531646231,0.224684645967589,-2.92349075108561E-16));
#16197=DIRECTION('',(2.99720887206891E-16,-1.29778303242547E-18,-1.));
#16198=DIRECTION('center_axis',(-0.974431531646231,0.224684645967588,-2.92349075108561E-16));
#16199=DIRECTION('ref_axis',(-2.99720887206891E-16,1.29778303242548E-18,
1.));
#16200=DIRECTION('',(2.99720887206891E-16,-1.29778303242547E-18,-1.));
#16201=DIRECTION('center_axis',(2.99720887206891E-16,-1.29778303242547E-18,
-1.));
#16202=DIRECTION('ref_axis',(-0.974431531646231,0.224684645967589,-2.92349075108561E-16));
#16203=DIRECTION('',(2.99720887206891E-16,-1.29778303242547E-18,-1.));
#16204=DIRECTION('center_axis',(-0.224684645967588,-0.974431531646231,-6.6078080723141E-17));
#16205=DIRECTION('ref_axis',(2.99720887206891E-16,-1.29778303242548E-18,
-1.));
#16206=DIRECTION('',(2.99720887206891E-16,-1.29778303242547E-18,-1.));
#16207=DIRECTION('center_axis',(2.99720887206891E-16,-1.29778303242547E-18,
-1.));
#16208=DIRECTION('ref_axis',(-0.974431531646231,0.224684645967589,-2.92349075108561E-16));
#16209=DIRECTION('',(2.99720887206891E-16,-1.29778303242547E-18,-1.));
#16210=DIRECTION('center_axis',(0.974431531646231,-0.224684645967588,2.92349075108561E-16));
#16211=DIRECTION('ref_axis',(2.99720887206891E-16,-1.29778303242548E-18,
-1.));
#16212=DIRECTION('',(2.99720887206891E-16,-1.29778303242547E-18,-1.));
#16213=DIRECTION('center_axis',(2.99720887206891E-16,-1.29778303242547E-18,
-1.));
#16214=DIRECTION('ref_axis',(-0.974431531646231,0.224684645967589,-2.92349075108561E-16));
#16215=DIRECTION('',(2.99720887206891E-16,-1.29778303242547E-18,-1.));
#16216=DIRECTION('center_axis',(0.224684645967588,0.974431531646231,6.6078080723141E-17));
#16217=DIRECTION('ref_axis',(-2.99720887206891E-16,1.29778303242548E-18,
1.));
#16218=DIRECTION('',(-2.99720887206891E-16,1.29778303242547E-18,1.));
#16219=DIRECTION('',(-0.689027143829042,0.15887603679218,-0.707106781186549));
#16220=DIRECTION('',(0.689027143829045,-0.158876036792181,-0.707106781186546));
#16221=DIRECTION('',(-2.99720887206891E-16,1.29778303242547E-18,1.));
#16222=DIRECTION('center_axis',(0.224684645967588,0.974431531646231,6.6078080723141E-17));
#16223=DIRECTION('ref_axis',(-1.48467301734967E-17,-6.43885654072936E-17,
1.));
#16224=DIRECTION('center_axis',(-0.974431531646231,0.224684645967588,-2.92349075108561E-16));
#16225=DIRECTION('ref_axis',(-2.99720887206891E-16,1.29778303242548E-18,
1.));
#16226=DIRECTION('',(-0.224684645967588,-0.974431531646231,-6.60780807231409E-17));
#16227=DIRECTION('',(-0.224684645967588,-0.974431531646231,-6.60780807231409E-17));
#16228=DIRECTION('center_axis',(-0.224684645967588,-0.974431531646231,-6.6078080723141E-17));
#16229=DIRECTION('ref_axis',(1.48467301734967E-17,6.43885654072935E-17,
-1.));
#16230=DIRECTION('',(-0.224684645967588,-0.974431531646231,-6.60780807231409E-17));
#16231=DIRECTION('center_axis',(-0.974431531646231,0.224684645967588,-2.92349075108561E-16));
#16232=DIRECTION('ref_axis',(-2.99720887206891E-16,1.29778303242548E-18,
1.));
#16233=DIRECTION('',(0.224684645967588,0.974431531646231,6.60780807231409E-17));
#16234=DIRECTION('center_axis',(0.974431531646231,-0.224684645967588,2.92349075108561E-16));
#16235=DIRECTION('ref_axis',(2.99720887206891E-16,-1.29778303242548E-18,
-1.));
#16236=DIRECTION('',(0.224684645967588,0.974431531646231,6.60780807231409E-17));
#16237=DIRECTION('',(-0.224684645967588,-0.974431531646231,-6.60780807231409E-17));
#16238=DIRECTION('center_axis',(-0.224684645967588,-0.974431531646231,-6.6078080723141E-17));
#16239=DIRECTION('ref_axis',(1.48467301734967E-17,6.43885654072935E-17,
-1.));
#16240=DIRECTION('',(-0.224684645967588,-0.974431531646231,-6.60780807231409E-17));
#16241=DIRECTION('center_axis',(0.974431531646231,-0.224684645967588,2.92349075108561E-16));
#16242=DIRECTION('ref_axis',(2.99720887206891E-16,-1.29778303242548E-18,
-1.));
#16243=DIRECTION('',(-0.224684645967588,-0.974431531646231,-6.60780807231409E-17));
#16244=DIRECTION('center_axis',(-0.689027143829045,0.158876036792181,0.707106781186546));
#16245=DIRECTION('ref_axis',(-0.224684645967588,-0.974431531646231,-5.55111512312579E-17));
#16246=DIRECTION('center_axis',(0.689027143829043,-0.15887603679218,0.707106781186549));
#16247=DIRECTION('ref_axis',(-0.224684645967588,-0.974431531646231,-5.55111512312579E-17));
#16248=DIRECTION('center_axis',(-0.689027143829045,0.158876036792181,0.707106781186546));
#16249=DIRECTION('ref_axis',(0.224684645967588,0.974431531646231,6.93889390390723E-17));
#16250=DIRECTION('center_axis',(0.689027143829043,-0.15887603679218,0.707106781186549));
#16251=DIRECTION('ref_axis',(0.224684645967588,0.974431531646231,5.55111512312579E-17));
#16252=DIRECTION('axis',(0.,0.,1.));
#16253=DIRECTION('refdir',(1.,0.,0.));
#16254=DIRECTION('',(0.487956526058392,0.511760784630642,0.707106306004447));
#16255=DIRECTION('',(0.487956174314074,0.51176044158493,-0.707106797009879));
#16256=DIRECTION('',(-0.487954254662986,-0.511762949542871,0.70710630659857));
#16257=DIRECTION('',(-0.487956174313991,-0.511760441584974,-0.707106797009905));
#16258=DIRECTION('center_axis',(-0.690074255005153,-0.72373857336685,7.51590717679369E-17));
#16259=DIRECTION('ref_axis',(-5.18653404571379E-17,-5.43955193769033E-17,
-1.));
#16260=DIRECTION('',(-0.690074255005153,-0.72373857336685,7.51590717679369E-17));
#16261=DIRECTION('center_axis',(8.42524722855705E-17,2.35148579188733E-17,
1.));
#16262=DIRECTION('ref_axis',(-0.690074255005155,-0.723738573366849,7.5159071767937E-17));
#16263=DIRECTION('center_axis',(8.42524722855705E-17,2.35148579188733E-17,
1.));
#16264=DIRECTION('ref_axis',(-0.690074255005155,-0.723738573366849,7.5159071767937E-17));
#16265=DIRECTION('',(-0.345037127502578,-0.361869286683425,-0.866025403784438));
#16266=DIRECTION('center_axis',(8.42524722855705E-17,2.35148579188733E-17,
1.));
#16267=DIRECTION('ref_axis',(-0.690074255005155,-0.723738573366848,7.5159071767937E-17));
#16268=DIRECTION('center_axis',(8.42524722855705E-17,2.35148579188733E-17,
1.));
#16269=DIRECTION('ref_axis',(-0.690074255005155,-0.723738573366849,7.5159071767937E-17));
#16270=DIRECTION('center_axis',(8.42524722855705E-17,2.35148579188733E-17,
1.));
#16271=DIRECTION('ref_axis',(-0.690074255005155,-0.723738573366849,7.5159071767937E-17));
#16272=DIRECTION('center_axis',(8.42524722855705E-17,2.35148579188733E-17,
1.));
#16273=DIRECTION('ref_axis',(-0.690074255005155,-0.723738573366849,7.5159071767937E-17));
#16274=DIRECTION('',(-8.42524722855704E-17,-2.35148579188733E-17,-1.));
#16275=DIRECTION('center_axis',(8.42524722855705E-17,2.35148579188733E-17,
1.));
#16276=DIRECTION('ref_axis',(-0.690074255005153,-0.723738573366849,0.));
#16277=DIRECTION('center_axis',(8.42524722855705E-17,2.35148579188733E-17,
1.));
#16278=DIRECTION('ref_axis',(-0.690074255005155,-0.723738573366848,7.5159071767937E-17));
#16279=DIRECTION('center_axis',(0.723738573366851,-0.690074255005152,-4.47497660346704E-17));
#16280=DIRECTION('ref_axis',(0.690074255005152,0.723738573366851,0.));
#16281=DIRECTION('center_axis',(8.42524722855705E-17,2.35148579188733E-17,
1.));
#16282=DIRECTION('ref_axis',(-0.690074255005154,-0.723738573366849,7.51590717679369E-17));
#16283=DIRECTION('center_axis',(8.42524722855705E-17,2.35148579188733E-17,
1.));
#16284=DIRECTION('ref_axis',(-0.690074255005154,-0.723738573366849,7.51590717679369E-17));
#16285=DIRECTION('center_axis',(8.42524722855705E-17,2.35148579188733E-17,
1.));
#16286=DIRECTION('ref_axis',(-0.690074255005154,-0.723738573366849,7.51590717679369E-17));
#16287=DIRECTION('',(-8.42524722855705E-17,-2.35148579188733E-17,-1.));
#16288=DIRECTION('center_axis',(8.42524722855705E-17,2.35148579188733E-17,
1.));
#16289=DIRECTION('ref_axis',(-0.690074255005154,-0.723738573366849,7.51590717679369E-17));
#16290=DIRECTION('center_axis',(-8.42524722855705E-17,-2.35148579188733E-17,
-1.));
#16291=DIRECTION('ref_axis',(0.690074255005153,0.72373857336685,-7.51590717679369E-17));
#16292=DIRECTION('',(0.487956185236399,0.511760453033977,0.707106781186547));
#16293=DIRECTION('center_axis',(8.42524722855705E-17,2.35148579188733E-17,
1.));
#16294=DIRECTION('ref_axis',(-0.690074255005153,-0.72373857336685,7.51590717679369E-17));
#16295=DIRECTION('center_axis',(8.42524722855704E-17,2.35148579188733E-17,
1.));
#16296=DIRECTION('ref_axis',(-0.690074255005153,-0.72373857336685,7.51590717679369E-17));
#16297=DIRECTION('center_axis',(-8.42524722855704E-17,-2.35148579188733E-17,
-1.));
#16298=DIRECTION('ref_axis',(0.690074255005153,0.72373857336685,-7.51590717679369E-17));
#16299=DIRECTION('center_axis',(-8.42524722855704E-17,-2.35148579188733E-17,
-1.));
#16300=DIRECTION('ref_axis',(0.690074255005153,0.72373857336685,-7.51590717679369E-17));
#16301=DIRECTION('',(0.0359217337292158,-0.706194237483284,0.707106306004472));
#16302=DIRECTION('',(0.0359217266067779,-0.706193746205675,-0.707106797009888));
#16303=DIRECTION('',(-0.0359248674940963,0.706194077477286,0.707106306598617));
#16304=DIRECTION('',(-0.0359217266067779,0.706193746205675,-0.707106797009888));
#16305=DIRECTION('center_axis',(-0.0508009940819139,0.998708795896126,-1.92022413686896E-17));
#16306=DIRECTION('ref_axis',(9.7549295013028E-19,-1.91774473558307E-17,
-1.));
#16307=DIRECTION('',(-0.0508009940819138,0.998708795896126,-1.92022413686896E-17));
#16308=DIRECTION('center_axis',(8.42672643859301E-17,2.35134628477836E-17,
1.));
#16309=DIRECTION('ref_axis',(-0.0508009940819175,0.998708795896126,-1.92022413686893E-17));
#16310=DIRECTION('center_axis',(8.42672643859301E-17,2.35134628477836E-17,
1.));
#16311=DIRECTION('ref_axis',(-0.0508009940819175,0.998708795896126,-1.92022413686893E-17));
#16312=DIRECTION('',(-0.0254004970409589,0.499354397948064,-0.866025403784438));
#16313=DIRECTION('center_axis',(8.42672643859301E-17,2.35134628477836E-17,
1.));
#16314=DIRECTION('ref_axis',(-0.0508009940819193,0.998708795896126,-1.92022413686891E-17));
#16315=DIRECTION('center_axis',(8.42672643859301E-17,2.35134628477836E-17,
1.));
#16316=DIRECTION('ref_axis',(-0.0508009940819175,0.998708795896126,-1.92022413686893E-17));
#16317=DIRECTION('center_axis',(8.42672643859301E-17,2.35134628477836E-17,
1.));
#16318=DIRECTION('ref_axis',(-0.0508009940819175,0.998708795896126,-1.92022413686893E-17));
#16319=DIRECTION('center_axis',(8.42672643859301E-17,2.35134628477836E-17,
1.));
#16320=DIRECTION('ref_axis',(-0.0508009940819175,0.998708795896126,-1.92022413686893E-17));
#16321=DIRECTION('',(-8.42672643859301E-17,-2.35134628477836E-17,-1.));
#16322=DIRECTION('center_axis',(8.42672643859301E-17,2.35134628477836E-17,
1.));
#16323=DIRECTION('ref_axis',(-0.0508009940819075,0.998708795896126,0.));
#16324=DIRECTION('center_axis',(8.42672643859301E-17,2.35134628477836E-17,
1.));
#16325=DIRECTION('ref_axis',(-0.0508009940819092,0.998708795896126,-1.920224136869E-17));
#16326=DIRECTION('center_axis',(-0.998708795896126,-0.0508009940819131,
8.53529654353083E-17));
#16327=DIRECTION('ref_axis',(0.0508009940819131,-0.998708795896126,0.));
#16328=DIRECTION('center_axis',(8.42672643859301E-17,2.35134628477836E-17,
1.));
#16329=DIRECTION('ref_axis',(-0.0508009940819137,0.998708795896126,-1.92022413686896E-17));
#16330=DIRECTION('center_axis',(8.42672643859301E-17,2.35134628477836E-17,
1.));
#16331=DIRECTION('ref_axis',(-0.0508009940819137,0.998708795896126,-1.92022413686896E-17));
#16332=DIRECTION('center_axis',(8.42672643859301E-17,2.35134628477836E-17,
1.));
#16333=DIRECTION('ref_axis',(-0.0508009940819137,0.998708795896126,-1.92022413686896E-17));
#16334=DIRECTION('',(-8.42672643859301E-17,-2.35134628477836E-17,-1.));
#16335=DIRECTION('center_axis',(8.42672643859301E-17,2.35134628477836E-17,
1.));
#16336=DIRECTION('ref_axis',(-0.0508009940819137,0.998708795896126,-1.92022413686896E-17));
#16337=DIRECTION('center_axis',(-8.42672643859301E-17,-2.35134628477836E-17,
-1.));
#16338=DIRECTION('ref_axis',(0.0508009940819178,-0.998708795896126,1.92022413686892E-17));
#16339=DIRECTION('',(0.0359217274063417,-0.706193762008803,0.707106781186547));
#16340=DIRECTION('center_axis',(8.42672643859301E-17,2.35134628477836E-17,
1.));
#16341=DIRECTION('ref_axis',(-0.0508009940819178,0.998708795896126,-1.92022413686892E-17));
#16342=DIRECTION('center_axis',(8.42672643859301E-17,2.35134628477836E-17,
1.));
#16343=DIRECTION('ref_axis',(-0.0508009940819138,0.998708795896126,-1.92022413686896E-17));
#16344=DIRECTION('center_axis',(-8.42672643859301E-17,-2.35134628477836E-17,
-1.));
#16345=DIRECTION('ref_axis',(0.0508009940819138,-0.998708795896126,1.92022413686896E-17));
#16346=DIRECTION('center_axis',(-8.42672643859301E-17,-2.35134628477836E-17,
-1.));
#16347=DIRECTION('ref_axis',(0.0508009940819138,-0.998708795896126,1.92022413686896E-17));
#16348=DIRECTION('axis',(0.,0.,1.));
#16349=DIRECTION('refdir',(1.,0.,0.));
#16350=DIRECTION('center_axis',(-0.179306265355413,-0.00912071322752245,
0.983751023274952));
#16351=DIRECTION('ref_axis',(-0.0508009940819341,0.998708795896125,0.));
#16352=DIRECTION('center_axis',(-0.7306405634129,0.670855725914997,-0.126952597857399));
#16353=DIRECTION('ref_axis',(-0.179306265355412,-0.00912071322752053,0.983751023274952));
#16354=DIRECTION('center_axis',(0.179306265355413,0.00912071322752245,-0.983751023274952));
#16355=DIRECTION('ref_axis',(-0.0508009940819232,0.998708795896125,7.43409742643818E-16));
#16356=DIRECTION('center_axis',(0.658797108600206,0.741531798102594,0.1269525978574));
#16357=DIRECTION('ref_axis',(-0.179306265355399,-0.00912071322753601,0.983751023274955));
#16358=DIRECTION('center_axis',(-0.179306265355413,-0.00912071322752245,
0.983751023274952));
#16359=DIRECTION('ref_axis',(-0.0508009940819344,0.998708795896125,0.));
#16360=DIRECTION('center_axis',(-0.730640563412892,0.670855725915006,-0.126952597857398));
#16361=DIRECTION('ref_axis',(-0.179306265355412,-0.00912071322752053,0.983751023274952));
#16362=DIRECTION('center_axis',(0.179306265355413,0.00912071322752245,-0.983751023274952));
#16363=DIRECTION('ref_axis',(-0.0508009940819232,0.998708795896125,7.43409742643818E-16));
#16364=DIRECTION('center_axis',(0.0508009940819268,-0.998708795896125,-7.81461095279302E-17));
#16365=DIRECTION('ref_axis',(-0.179306265355397,-0.00912071322752166,0.983751023274955));
#16366=DIRECTION('center_axis',(0.,0.,1.));
#16367=DIRECTION('ref_axis',(1.,0.,0.));
#16368=DIRECTION('center_axis',(0.658797108600203,0.741531798102596,0.126952597857399));
#16369=DIRECTION('ref_axis',(-0.730640563412887,0.670855725915008,-0.126952597857418));
#16370=DIRECTION('center_axis',(0.658797108600203,0.741531798102596,0.126952597857399));
#16371=DIRECTION('ref_axis',(-0.730640563412887,0.670855725915008,-0.126952597857418));
#16372=DIRECTION('center_axis',(0.,-1.,0.));
#16373=DIRECTION('ref_axis',(-1.,0.,0.));
#16374=DIRECTION('center_axis',(1.,0.,0.));
#16375=DIRECTION('ref_axis',(0.,-1.,0.));
#16376=DIRECTION('center_axis',(-0.0508009940819267,0.998708795896125,1.00133183721819E-16));
#16377=DIRECTION('ref_axis',(0.98248079991651,0.0499755299114802,0.17953808566842));
#16378=DIRECTION('center_axis',(-0.0508009940819267,0.998708795896125,1.00133183721819E-16));
#16379=DIRECTION('ref_axis',(0.98248079991651,0.0499755299114802,0.17953808566842));
#16380=DIRECTION('center_axis',(0.,0.,1.));
#16381=DIRECTION('ref_axis',(0.,1.,0.));
#16382=DIRECTION('center_axis',(-0.658797108600203,-0.741531798102596,-0.126952597857399));
#16383=DIRECTION('ref_axis',(-0.730640563412892,0.670855725915008,-0.126952597857391));
#16384=DIRECTION('',(0.658797108600203,0.741531798102596,0.126952597857399));
#16385=DIRECTION('center_axis',(0.658797108600207,0.741531798102593,0.1269525978574));
#16386=DIRECTION('ref_axis',(-0.179306265355399,-0.00912071322753602,0.983751023274955));
#16387=DIRECTION('center_axis',(0.658797108600207,0.741531798102593,0.1269525978574));
#16388=DIRECTION('ref_axis',(-0.179306265355399,-0.00912071322753602,0.983751023274955));
#16389=DIRECTION('center_axis',(0.730640563412901,-0.670855725914996,0.126952597857399));
#16390=DIRECTION('ref_axis',(-0.658797108600193,-0.741531798102606,-0.126952597857392));
#16391=DIRECTION('center_axis',(-0.730640563412901,0.670855725914996,-0.126952597857399));
#16392=DIRECTION('ref_axis',(-0.179306265355412,-0.00912071322752052,0.983751023274952));
#16393=DIRECTION('',(-0.730640563412901,0.670855725914996,-0.126952597857399));
#16394=DIRECTION('center_axis',(-0.730640563412901,0.670855725914996,-0.126952597857399));
#16395=DIRECTION('ref_axis',(-0.179306265355412,-0.00912071322752052,0.983751023274952));
#16396=DIRECTION('center_axis',(-0.658797108600206,-0.741531798102594,-0.1269525978574));
#16397=DIRECTION('ref_axis',(-0.73064056341289,0.67085572591501,-0.126952597857391));
#16398=DIRECTION('',(0.658797108600206,0.741531798102594,0.1269525978574));
#16399=DIRECTION('center_axis',(0.658797108600204,0.741531798102595,0.126952597857399));
#16400=DIRECTION('ref_axis',(-0.179306265355399,-0.00912071322753602,0.983751023274955));
#16401=DIRECTION('center_axis',(0.658797108600204,0.741531798102595,0.126952597857399));
#16402=DIRECTION('ref_axis',(-0.179306265355399,-0.00912071322753602,0.983751023274955));
#16403=DIRECTION('center_axis',(0.730640563412891,-0.670855725915007,0.126952597857398));
#16404=DIRECTION('ref_axis',(-0.658797108600205,-0.741531798102597,-0.126952597857384));
#16405=DIRECTION('center_axis',(-0.730640563412891,0.670855725915007,-0.126952597857398));
#16406=DIRECTION('ref_axis',(-0.179306265355412,-0.00912071322752052,0.983751023274952));
#16407=DIRECTION('',(-0.730640563412891,0.670855725915007,-0.126952597857398));
#16408=DIRECTION('center_axis',(-0.730640563412891,0.670855725915007,-0.126952597857398));
#16409=DIRECTION('ref_axis',(-0.179306265355412,-0.00912071322752052,0.983751023274952));
#16410=DIRECTION('center_axis',(-0.0508009940819267,0.998708795896125,1.00133183721819E-16));
#16411=DIRECTION('ref_axis',(0.98248079991651,0.0499755299114802,0.17953808566842));
#16412=DIRECTION('',(0.0508009940819267,-0.998708795896125,-1.00133183721819E-16));
#16413=DIRECTION('center_axis',(-0.628842175749928,0.599591913317124,0.49502227776415));
#16414=DIRECTION('ref_axis',(-0.690074255005139,-0.723738573366864,0.));
#16415=DIRECTION('center_axis',(-0.234623360105886,-0.753309635298807,0.614391139469477));
#16416=DIRECTION('ref_axis',(-0.628842175749927,0.599591913317124,0.495022277764151));
#16417=DIRECTION('center_axis',(0.628842175749928,-0.599591913317124,-0.49502227776415));
#16418=DIRECTION('ref_axis',(-0.69007425500514,-0.723738573366862,5.49585130476149E-16));
#16419=DIRECTION('center_axis',(-0.741289010366885,-0.270211270769156,-0.614391139469478));
#16420=DIRECTION('ref_axis',(-0.628842175749928,0.599591913317122,0.495022277764152));
#16421=DIRECTION('center_axis',(-0.628842175749928,0.599591913317124,0.49502227776415));
#16422=DIRECTION('ref_axis',(-0.690074255005139,-0.723738573366864,0.));
#16423=DIRECTION('center_axis',(-0.234623360105896,-0.75330963529881,0.614391139469469));
#16424=DIRECTION('ref_axis',(-0.628842175749927,0.599591913317124,0.495022277764151));
#16425=DIRECTION('center_axis',(0.628842175749928,-0.599591913317124,-0.49502227776415));
#16426=DIRECTION('ref_axis',(-0.69007425500514,-0.723738573366862,5.49585130476149E-16));
#16427=DIRECTION('center_axis',(0.69007425500514,0.723738573366862,-1.81566217392232E-16));
#16428=DIRECTION('ref_axis',(-0.628842175749927,0.599591913317123,0.495022277764153));
#16429=DIRECTION('center_axis',(0.,0.,1.));
#16430=DIRECTION('ref_axis',(1.,0.,0.));
#16431=DIRECTION('center_axis',(-0.741289010366885,-0.270211270769158,-0.614391139469476));
#16432=DIRECTION('ref_axis',(-0.234623360105902,-0.753309635298806,0.614391139469472));
#16433=DIRECTION('center_axis',(-0.741289010366885,-0.270211270769158,-0.614391139469476));
#16434=DIRECTION('ref_axis',(-0.234623360105902,-0.753309635298806,0.614391139469472));
#16435=DIRECTION('center_axis',(0.,-1.,0.));
#16436=DIRECTION('ref_axis',(-1.,0.,0.));
#16437=DIRECTION('center_axis',(1.,0.,0.));
#16438=DIRECTION('ref_axis',(0.,-1.,0.));
#16439=DIRECTION('center_axis',(-0.69007425500514,-0.723738573366862,7.51590717680294E-17));
#16440=DIRECTION('ref_axis',(-0.358266717093849,0.341602129539051,-0.868880282039581));
#16441=DIRECTION('center_axis',(0.,0.,1.));
#16442=DIRECTION('ref_axis',(0.,1.,0.));
#16443=DIRECTION('center_axis',(-0.69007425500514,-0.723738573366862,7.51590717680294E-17));
#16444=DIRECTION('ref_axis',(-0.358266717093849,0.341602129539051,-0.868880282039581));
#16445=DIRECTION('center_axis',(0.741289010366885,0.270211270769158,0.614391139469476));
#16446=DIRECTION('ref_axis',(-0.234623360105893,-0.753309635298815,0.614391139469465));
#16447=DIRECTION('',(-0.741289010366885,-0.270211270769158,-0.614391139469476));
#16448=DIRECTION('center_axis',(-0.741289010366884,-0.270211270769154,-0.614391139469479));
#16449=DIRECTION('ref_axis',(-0.628842175749928,0.599591913317122,0.495022277764152));
#16450=DIRECTION('center_axis',(-0.741289010366884,-0.270211270769154,-0.614391139469479));
#16451=DIRECTION('ref_axis',(-0.628842175749928,0.599591913317122,0.495022277764152));
#16452=DIRECTION('center_axis',(0.234623360105886,0.753309635298807,-0.614391139469477));
#16453=DIRECTION('ref_axis',(0.741289010366886,0.270211270769172,0.614391139469469));
#16454=DIRECTION('center_axis',(-0.234623360105886,-0.753309635298807,0.614391139469477));
#16455=DIRECTION('ref_axis',(-0.628842175749927,0.599591913317124,0.495022277764151));
#16456=DIRECTION('',(-0.234623360105886,-0.753309635298807,0.614391139469477));
#16457=DIRECTION('center_axis',(-0.234623360105886,-0.753309635298807,0.614391139469477));
#16458=DIRECTION('ref_axis',(-0.628842175749927,0.599591913317124,0.495022277764151));
#16459=DIRECTION('center_axis',(0.741289010366884,0.270211270769155,0.614391139469478));
#16460=DIRECTION('ref_axis',(-0.234623360105895,-0.753309635298815,0.614391139469463));
#16461=DIRECTION('',(-0.741289010366885,-0.270211270769155,-0.614391139469478));
#16462=DIRECTION('center_axis',(-0.741289010366885,-0.270211270769157,-0.614391139469477));
#16463=DIRECTION('ref_axis',(-0.628842175749928,0.599591913317122,0.495022277764152));
#16464=DIRECTION('center_axis',(-0.741289010366885,-0.270211270769157,-0.614391139469477));
#16465=DIRECTION('ref_axis',(-0.628842175749928,0.599591913317122,0.495022277764152));
#16466=DIRECTION('center_axis',(0.234623360105896,0.75330963529881,-0.614391139469469));
#16467=DIRECTION('ref_axis',(0.741289010366884,0.27021127076916,0.614391139469476));
#16468=DIRECTION('center_axis',(-0.234623360105896,-0.75330963529881,0.614391139469469));
#16469=DIRECTION('ref_axis',(-0.628842175749927,0.599591913317124,0.495022277764151));
#16470=DIRECTION('',(-0.234623360105896,-0.75330963529881,0.614391139469469));
#16471=DIRECTION('center_axis',(-0.234623360105896,-0.75330963529881,0.614391139469469));
#16472=DIRECTION('ref_axis',(-0.628842175749927,0.599591913317124,0.495022277764151));
#16473=DIRECTION('center_axis',(-0.69007425500514,-0.723738573366862,7.51590717680294E-17));
#16474=DIRECTION('ref_axis',(-0.358266717093849,0.341602129539051,-0.868880282039581));
#16475=DIRECTION('',(0.69007425500514,0.723738573366862,-7.51590717680294E-17));
#16476=DIRECTION('',(0.,0.,1.));
#16477=DIRECTION('',(1.,0.,0.));
#16478=DIRECTION('',(0.,0.,1.));
#16479=DIRECTION('',(1.,0.,0.));
#16480=DIRECTION('',(0.,0.,1.));
#16481=DIRECTION('',(1.,0.,0.));
#16482=DIRECTION('',(0.,0.,1.));
#16483=DIRECTION('',(1.,0.,0.));
#16484=DIRECTION('',(0.,0.,1.));
#16485=DIRECTION('',(1.,0.,0.));
#16486=DIRECTION('',(0.,0.,1.));
#16487=DIRECTION('',(1.,0.,0.));
#16488=DIRECTION('',(0.,0.,1.));
#16489=DIRECTION('',(1.,0.,0.));
#16490=DIRECTION('axis',(0.,0.,1.));
#16491=DIRECTION('refdir',(1.,0.,0.));
#16492=DIRECTION('axis',(0.,0.,1.));
#16493=DIRECTION('refdir',(1.,0.,0.));
#16494=DIRECTION('center_axis',(-2.73022310513781E-17,4.45132926068947E-17,
-1.));
#16495=DIRECTION('ref_axis',(0.852431871234064,0.522838316216775,-3.69481375527776E-23));
#16496=DIRECTION('center_axis',(-2.73022310513781E-17,4.45132926068947E-17,
-1.));
#16497=DIRECTION('ref_axis',(0.852431871234064,0.522838316216775,-3.69481375527776E-23));
#16498=DIRECTION('',(-2.73022310513781E-17,4.45132926068947E-17,-1.));
#16499=DIRECTION('center_axis',(-2.73022310513781E-17,4.45132926068947E-17,
-1.));
#16500=DIRECTION('ref_axis',(0.852431871234064,0.522838316216775,-3.69481375527776E-23));
#16501=DIRECTION('center_axis',(-2.73022310513781E-17,4.45132926068947E-17,
-1.));
#16502=DIRECTION('ref_axis',(0.852431871234061,0.522838316216779,-3.69481373062586E-23));
#16503=DIRECTION('center_axis',(-2.73022310513781E-17,4.45132926068947E-17,
-1.));
#16504=DIRECTION('ref_axis',(0.852431871234061,0.522838316216779,-3.69481373062586E-23));
#16505=DIRECTION('',(-2.73022310513781E-17,4.45132926068947E-17,-1.));
#16506=DIRECTION('center_axis',(-2.73022310513781E-17,4.45132926068947E-17,
-1.));
#16507=DIRECTION('ref_axis',(0.852431871234061,0.522838316216779,-3.69481373062586E-23));
#16508=DIRECTION('center_axis',(2.73022310513781E-17,-4.45132926068947E-17,
1.));
#16509=DIRECTION('ref_axis',(-0.852431871234064,-0.522838316216775,3.69481375527776E-23));
#16510=DIRECTION('center_axis',(-2.73022310513781E-17,4.45132926068947E-17,
-1.));
#16511=DIRECTION('ref_axis',(0.852431871234064,0.522838316216775,-3.69481375527776E-23));
#16512=DIRECTION('',(2.73022310513781E-17,-4.45132926068947E-17,1.));
#16513=DIRECTION('center_axis',(-2.73022310513781E-17,4.45132926068947E-17,
-1.));
#16514=DIRECTION('ref_axis',(0.852431871234064,0.522838316216775,-3.69481375527776E-23));
#16515=DIRECTION('center_axis',(2.73022310513781E-17,-4.45132926068947E-17,
1.));
#16516=DIRECTION('ref_axis',(-0.852431871234061,-0.522838316216779,3.69481373062586E-23));
#16517=DIRECTION('center_axis',(-2.73022310513781E-17,4.45132926068947E-17,
-1.));
#16518=DIRECTION('ref_axis',(0.852431871234061,0.522838316216779,-3.69481373062586E-23));
#16519=DIRECTION('',(2.73022310513781E-17,-4.45132926068947E-17,1.));
#16520=DIRECTION('center_axis',(-2.73022310513781E-17,4.45132926068947E-17,
-1.));
#16521=DIRECTION('ref_axis',(0.852431871234061,0.522838316216779,-3.69481373062586E-23));
#16522=DIRECTION('center_axis',(-0.852431871234063,-0.522838316216777,-2.44136686633116E-17));
#16523=DIRECTION('ref_axis',(-0.522838316216777,0.852431871234063,2.31111593326468E-32));
#16524=DIRECTION('center_axis',(0.852431871234063,0.522838316216777,2.44136686633116E-17));
#16525=DIRECTION('ref_axis',(0.522838316216777,-0.852431871234063,-2.31111593326468E-32));
#16526=DIRECTION('',(-0.852431871234063,-0.522838316216777,-2.44136686633116E-17));
#16527=DIRECTION('center_axis',(-0.852431871234063,-0.522838316216777,-2.44136686633116E-17));
#16528=DIRECTION('ref_axis',(-0.522838316216777,0.852431871234063,2.31111593326468E-32));
#16529=DIRECTION('',(0.852431871234063,0.522838316216777,2.44136686633116E-17));
#16530=DIRECTION('center_axis',(0.852431871234063,0.522838316216777,2.44136686633116E-17));
#16531=DIRECTION('ref_axis',(0.522838316216777,-0.852431871234063,3.23556230657056E-32));
#16532=DIRECTION('',(0.852431871234063,0.522838316216777,2.44136686633116E-17));
#16533=DIRECTION('center_axis',(0.852431871234063,0.522838316216777,2.44136686633116E-17));
#16534=DIRECTION('ref_axis',(0.522838316216777,-0.852431871234063,-2.31111593326468E-32));
#16535=DIRECTION('',(0.852431871234063,0.522838316216777,2.44136686633116E-17));
#16536=DIRECTION('center_axis',(0.852431871234063,0.522838316216777,2.44136686633116E-17));
#16537=DIRECTION('ref_axis',(0.522838316216777,-0.852431871234063,3.23556230657056E-32));
#16538=DIRECTION('',(-0.852431871234063,-0.522838316216777,-2.44136686633116E-17));
#16539=DIRECTION('center_axis',(-0.852431871234063,-0.522838316216777,-2.44136686633116E-17));
#16540=DIRECTION('ref_axis',(-0.522838316216777,0.852431871234063,2.31111593326468E-32));
#16541=DIRECTION('center_axis',(-0.852431871234063,-0.522838316216777,-2.44136686633116E-17));
#16542=DIRECTION('ref_axis',(-0.522838316216777,0.852431871234063,1.54074395550979E-32));
#16543=DIRECTION('center_axis',(0.852431871234063,0.522838316216777,2.44136686633116E-17));
#16544=DIRECTION('ref_axis',(0.522838316216777,-0.852431871234063,-1.54074395550979E-32));
#16545=DIRECTION('',(0.852431871234063,0.522838316216777,2.44136686633116E-17));
#16546=DIRECTION('center_axis',(-0.852431871234063,-0.522838316216777,-2.44136686633116E-17));
#16547=DIRECTION('ref_axis',(0.522838316216777,-0.852431871234063,-1.54074395550979E-32));
#16548=DIRECTION('',(0.852431871234063,0.522838316216777,2.44136686633116E-17));
#16549=DIRECTION('center_axis',(0.852431871234063,0.522838316216777,2.44136686633116E-17));
#16550=DIRECTION('ref_axis',(0.522838316216777,-0.852431871234063,-1.54074395550979E-32));
#16551=DIRECTION('center_axis',(-0.852431871234063,-0.522838316216777,-2.44136686633116E-17));
#16552=DIRECTION('ref_axis',(-0.522838316216777,0.852431871234063,1.54074395550979E-32));
#16553=DIRECTION('',(0.852431871234063,0.522838316216777,2.44136686633116E-17));
#16554=DIRECTION('center_axis',(0.852431871234063,0.522838316216777,2.44136686633116E-17));
#16555=DIRECTION('ref_axis',(0.522838316216777,-0.852431871234063,-1.54074395550979E-32));
#16556=DIRECTION('center_axis',(-0.852431871234063,-0.522838316216777,-2.44136686633116E-17));
#16557=DIRECTION('ref_axis',(-0.522838316216777,0.852431871234063,1.54074395550979E-32));
#16558=DIRECTION('center_axis',(-0.852431871234063,-0.522838316216777,-2.44136686633116E-17));
#16559=DIRECTION('ref_axis',(-0.522838316216777,0.852431871234063,1.54074395550979E-32));
#16560=DIRECTION('',(-0.852431871234063,-0.522838316216777,-2.44136686633116E-17));
#16561=DIRECTION('center_axis',(-0.852431871234063,-0.522838316216777,-2.44136686633116E-17));
#16562=DIRECTION('ref_axis',(0.522838316216777,-0.852431871234063,-1.54074395550979E-32));
#16563=DIRECTION('',(0.852431871234063,0.522838316216777,2.44136686633116E-17));
#16564=DIRECTION('center_axis',(-0.522838316216777,0.852431871234063,1.10549867763274E-16));
#16565=DIRECTION('ref_axis',(0.852431871234063,0.522838316216777,2.44136686633116E-17));
#16566=DIRECTION('',(-0.852431871234063,-0.522838316216777,-2.44136686633116E-17));
#16567=DIRECTION('',(2.73022310513781E-17,-4.45132926068947E-17,1.));
#16568=DIRECTION('',(-0.852431871234063,-0.522838316216777,-2.44136686633116E-17));
#16569=DIRECTION('',(2.73022310513781E-17,-4.45132926068947E-17,1.));
#16570=DIRECTION('center_axis',(0.522838316216777,-0.852431871234063,-1.10549867763274E-16));
#16571=DIRECTION('ref_axis',(-0.852431871234063,-0.522838316216777,-2.44136686633116E-17));
#16572=DIRECTION('',(2.73022310513781E-17,-4.45132926068947E-17,1.));
#16573=DIRECTION('',(-0.852431871234063,-0.522838316216777,-2.44136686633116E-17));
#16574=DIRECTION('',(-2.73022310513781E-17,4.45132926068947E-17,-1.));
#16575=DIRECTION('',(-0.852431871234063,-0.522838316216777,-2.44136686633116E-17));
#16576=DIRECTION('center_axis',(-0.852431871234063,-0.522838316216777,-2.44136686633116E-17));
#16577=DIRECTION('ref_axis',(-0.522838316216777,0.852431871234063,1.10549867763274E-16));
#16578=DIRECTION('',(0.522838316216777,-0.852431871234063,-1.10549867763274E-16));
#16579=DIRECTION('',(0.522838316216777,-0.852431871234063,-1.10549867763274E-16));
#16580=DIRECTION('center_axis',(0.852431871234063,0.522838316216777,2.44136686633116E-17));
#16581=DIRECTION('ref_axis',(0.522838316216777,-0.852431871234063,-1.10549867763274E-16));
#16582=DIRECTION('center_axis',(-0.852431871234063,-0.522838316216777,-2.44136686633116E-17));
#16583=DIRECTION('ref_axis',(-0.522838316216777,0.852431871234063,1.10549867763274E-16));
#16584=DIRECTION('',(0.522838316216777,-0.852431871234063,-1.10549867763274E-16));
#16585=DIRECTION('',(0.522838316216777,-0.852431871234063,-1.10549867763274E-16));
#16586=DIRECTION('',(2.73022310513781E-17,-4.45132926068947E-17,1.));
#16587=DIRECTION('center_axis',(-0.522838316216777,0.852431871234063,1.10549867763274E-16));
#16588=DIRECTION('ref_axis',(0.852431871234063,0.522838316216777,2.44136686633116E-17));
#16589=DIRECTION('',(-0.852431871234063,-0.522838316216777,-2.44136686633116E-17));
#16590=DIRECTION('',(2.73022310513781E-17,-4.45132926068947E-17,1.));
#16591=DIRECTION('',(-0.852431871234063,-0.522838316216777,-2.44136686633116E-17));
#16592=DIRECTION('center_axis',(-0.253157481559667,0.967425082128,1.12879065814692E-16));
#16593=DIRECTION('ref_axis',(0.967425082128,0.253157481559667,-8.69580248635087E-18));
#16594=DIRECTION('',(-0.967425082128,-0.253157481559667,8.69580248635087E-18));
#16595=DIRECTION('',(2.73022310513781E-17,-4.45132926068947E-17,1.));
#16596=DIRECTION('',(-0.967425082128,-0.253157481559667,8.69580248635087E-18));
#16597=DIRECTION('center_axis',(-0.852431871234063,-0.522838316216777,-2.44136686633116E-17));
#16598=DIRECTION('ref_axis',(-0.522838316216777,0.852431871234063,1.10549867763274E-16));
#16599=DIRECTION('',(0.522838316216777,-0.852431871234063,-1.10549867763274E-16));
#16600=DIRECTION('',(0.522838316216777,-0.852431871234063,-1.10549867763274E-16));
#16601=DIRECTION('center_axis',(-6.49121029325306E-18,5.72777133413967E-17,
-1.));
#16602=DIRECTION('ref_axis',(0.852431871234063,0.522838316216777,2.44136686633116E-17));
#16603=DIRECTION('center_axis',(-6.49121029325306E-18,5.72777133413967E-17,
-1.));
#16604=DIRECTION('ref_axis',(0.852431871234063,0.522838316216777,2.44136686633116E-17));
#16605=DIRECTION('center_axis',(0.852431871234063,0.522838316216777,2.44136686633116E-17));
#16606=DIRECTION('ref_axis',(0.522838316216777,-0.852431871234063,-1.10549867763274E-16));
#16607=DIRECTION('',(0.522838316216777,-0.852431871234063,-1.10549867763274E-16));
#16608=DIRECTION('',(-2.73022310513781E-17,4.45132926068947E-17,-1.));
#16609=DIRECTION('',(0.522838316216777,-0.852431871234063,-1.10549867763274E-16));
#16610=DIRECTION('center_axis',(0.522838316216777,-0.852431871234063,-1.10549867763274E-16));
#16611=DIRECTION('ref_axis',(-0.852431871234063,-0.522838316216777,-2.44136686633116E-17));
#16612=DIRECTION('',(-0.852431871234063,-0.522838316216777,-2.44136686633116E-17));
#16613=DIRECTION('',(-0.852431871234063,-0.522838316216777,-2.44136686633116E-17));
#16614=DIRECTION('',(-2.73022310513781E-17,4.45132926068947E-17,-1.));
#16615=DIRECTION('center_axis',(0.852431871234063,0.522838316216777,2.44136686633116E-17));
#16616=DIRECTION('ref_axis',(0.522838316216777,-0.852431871234063,-1.10549867763274E-16));
#16617=DIRECTION('',(0.522838316216777,-0.852431871234063,-1.10549867763274E-16));
#16618=DIRECTION('',(-2.73022310513781E-17,4.45132926068947E-17,-1.));
#16619=DIRECTION('',(0.522838316216777,-0.852431871234063,-1.10549867763274E-16));
#16620=DIRECTION('center_axis',(0.253157481559667,-0.967425082128,-1.12879065814692E-16));
#16621=DIRECTION('ref_axis',(-0.967425082128,-0.253157481559667,8.69580248635087E-18));
#16622=DIRECTION('',(-0.967425082128,-0.253157481559667,8.69580248635087E-18));
#16623=DIRECTION('',(-0.967425082128,-0.253157481559667,8.69580248635087E-18));
#16624=DIRECTION('center_axis',(6.49121029325306E-18,-5.72777133413967E-17,
1.));
#16625=DIRECTION('ref_axis',(0.852431871234063,0.522838316216777,2.44136686633116E-17));
#16626=DIRECTION('center_axis',(6.49121029325306E-18,-5.72777133413967E-17,
1.));
#16627=DIRECTION('ref_axis',(0.852431871234063,0.522838316216777,2.44136686633116E-17));
#16628=DIRECTION('center_axis',(0.852431871234063,0.522838316216777,2.44136686633116E-17));
#16629=DIRECTION('ref_axis',(-0.522838316216777,0.852431871234063,3.21624529935327E-16));
#16630=DIRECTION('center_axis',(0.852431871234063,0.522838316216777,2.44136686633116E-17));
#16631=DIRECTION('ref_axis',(0.522838316216777,-0.852431871234063,1.69481835106077E-32));
#16632=DIRECTION('center_axis',(0.852431871234063,0.522838316216777,2.44136686633116E-17));
#16633=DIRECTION('ref_axis',(0.522838316216777,-0.852431871234063,-6.16297582203915E-33));
#16634=DIRECTION('center_axis',(0.852431871234063,0.522838316216777,2.44136686633116E-17));
#16635=DIRECTION('ref_axis',(-0.522838316216777,0.852431871234063,1.89882151931499E-15));
#16636=DIRECTION('center_axis',(-0.852431871234063,-0.522838316216777,-2.44136686633116E-17));
#16637=DIRECTION('ref_axis',(0.522838316216777,-0.852431871234063,3.08148791101958E-33));
#16638=DIRECTION('center_axis',(0.852431871234063,0.522838316216777,2.44136686633116E-17));
#16639=DIRECTION('ref_axis',(0.522838316216777,-0.852431871234063,-1.10549867763274E-16));
#16640=DIRECTION('center_axis',(0.852431871234063,0.522838316216777,2.44136686633116E-17));
#16641=DIRECTION('ref_axis',(0.522838316216777,-0.852431871234063,-1.10549867763274E-16));
#16642=DIRECTION('center_axis',(0.852431871234063,0.522838316216777,2.44136686633116E-17));
#16643=DIRECTION('ref_axis',(-0.522838316216777,0.852431871234062,-3.45797464736582E-13));
#16644=DIRECTION('axis',(0.,0.,1.));
#16645=DIRECTION('refdir',(1.,0.,0.));
#16646=DIRECTION('center_axis',(0.852431871234063,0.522838316216777,2.44136686633116E-17));
#16647=DIRECTION('ref_axis',(0.522838316216774,-0.852431871234064,0.));
#16648=DIRECTION('center_axis',(0.852431871234063,0.522838316216777,2.44136686633116E-17));
#16649=DIRECTION('ref_axis',(0.522838316216777,-0.852431871234063,8.32001735975286E-32));
#16650=DIRECTION('center_axis',(0.852431871234063,0.522838316216777,2.44136686633116E-17));
#16651=DIRECTION('ref_axis',(0.522838316216777,-0.852431871234063,8.32001735975286E-32));
#16652=DIRECTION('center_axis',(-2.08109892623551E-17,-1.27644014166001E-17,
1.));
#16653=DIRECTION('ref_axis',(-0.522838316216777,0.852431871234063,0.));
#16654=DIRECTION('center_axis',(-0.852431871234063,-0.522838316216777,-2.44136686633116E-17));
#16655=DIRECTION('ref_axis',(0.522838316216777,-0.852431871234063,1.54074395550979E-32));
#16656=DIRECTION('center_axis',(-0.852431871234063,-0.522838316216777,-2.44136686633116E-17));
#16657=DIRECTION('ref_axis',(0.522838316216777,-0.852431871234063,1.54074395550979E-32));
#16658=DIRECTION('center_axis',(-0.852431871234063,-0.522838316216777,-2.44136686633116E-17));
#16659=DIRECTION('ref_axis',(-0.522838316216777,0.852431871234063,-8.32001735975286E-32));
#16660=DIRECTION('',(-0.852431871234063,-0.522838316216777,-2.44136686633116E-17));
#16661=DIRECTION('center_axis',(0.852431871234063,0.522838316216777,2.44136686633116E-17));
#16662=DIRECTION('ref_axis',(0.522838316216777,-0.852431871234063,-1.54074395550979E-32));
#16663=DIRECTION('center_axis',(-0.852431871234063,-0.522838316216777,-2.44136686633116E-17));
#16664=DIRECTION('ref_axis',(-0.522838316216777,0.852431871234063,-1.54074395550979E-32));
#16665=DIRECTION('center_axis',(0.852431871234063,0.522838316216777,2.44136686633116E-17));
#16666=DIRECTION('ref_axis',(0.522838316216777,-0.852431871234063,1.54074395550979E-32));
#16667=DIRECTION('',(0.852431871234063,0.522838316216777,2.44136686633116E-17));
#16668=DIRECTION('center_axis',(0.852431871234063,0.522838316216777,2.44136686633116E-17));
#16669=DIRECTION('ref_axis',(0.522838316216777,-0.852431871234063,-1.10549867763274E-16));
#16670=DIRECTION('axis',(0.,0.,1.));
#16671=DIRECTION('refdir',(1.,0.,0.));
#16672=DIRECTION('center_axis',(0.852431871234063,0.522838316216777,2.44136686633116E-17));
#16673=DIRECTION('ref_axis',(0.522838316216777,-0.852431871234062,0.));
#16674=DIRECTION('center_axis',(0.852431871234063,0.522838316216777,2.44136686633116E-17));
#16675=DIRECTION('ref_axis',(0.522838316216777,-0.852431871234063,1.84889274661175E-32));
#16676=DIRECTION('center_axis',(-2.08109892623551E-17,-1.27644014166001E-17,
1.));
#16677=DIRECTION('ref_axis',(-0.522838316216778,0.852431871234062,0.));
#16678=DIRECTION('center_axis',(-0.852431871234063,-0.522838316216777,-2.44136686633116E-17));
#16679=DIRECTION('ref_axis',(0.522838316216777,-0.852431871234063,-1.54074395550979E-32));
#16680=DIRECTION('center_axis',(-0.852431871234063,-0.522838316216777,-2.44136686633116E-17));
#16681=DIRECTION('ref_axis',(0.522838316216777,-0.852431871234063,-1.54074395550979E-32));
#16682=DIRECTION('center_axis',(0.852431871234063,0.522838316216777,2.44136686633116E-17));
#16683=DIRECTION('ref_axis',(0.522838316216777,-0.852431871234062,0.));
#16684=DIRECTION('center_axis',(0.852431871234063,0.522838316216777,2.44136686633116E-17));
#16685=DIRECTION('ref_axis',(0.522838316216777,-0.852431871234063,-1.54074395550979E-32));
#16686=DIRECTION('center_axis',(0.852431871234063,0.522838316216777,2.44136686633116E-17));
#16687=DIRECTION('ref_axis',(0.522838316216777,-0.852431871234063,-1.54074395550979E-32));
#16688=DIRECTION('center_axis',(-2.08109892623551E-17,-1.27644014166001E-17,
1.));
#16689=DIRECTION('ref_axis',(-0.522838316216776,0.852431871234063,0.));
#16690=DIRECTION('center_axis',(-0.852431871234063,-0.522838316216777,-2.44136686633116E-17));
#16691=DIRECTION('ref_axis',(0.522838316216777,-0.852431871234063,1.84889274661175E-32));
#16692=DIRECTION('center_axis',(-0.852431871234063,-0.522838316216777,-2.44136686633116E-17));
#16693=DIRECTION('ref_axis',(-0.522838316216777,0.852431871234063,1.54074395550979E-32));
#16694=DIRECTION('',(0.852431871234063,0.522838316216777,2.44136686633116E-17));
#16695=DIRECTION('center_axis',(-0.852431871234063,-0.522838316216777,-2.44136686633116E-17));
#16696=DIRECTION('ref_axis',(-0.522838316216777,0.852431871234063,-1.54074395550979E-32));
#16697=DIRECTION('center_axis',(0.852431871234063,0.522838316216777,2.44136686633116E-17));
#16698=DIRECTION('ref_axis',(-0.522838316216777,0.852431871234063,-1.69481835106077E-32));
#16699=DIRECTION('',(-0.852431871234063,-0.522838316216777,-2.44136686633116E-17));
#16700=DIRECTION('center_axis',(0.852431871234063,0.522838316216777,2.44136686633116E-17));
#16701=DIRECTION('ref_axis',(0.522838316216777,-0.852431871234063,1.54074395550979E-32));
#16702=DIRECTION('center_axis',(0.852431871234063,0.522838316216777,2.44136686633116E-17));
#16703=DIRECTION('ref_axis',(0.522838316216777,-0.852431871234063,-1.10549867763274E-16));
#16704=DIRECTION('center_axis',(0.852431871234063,0.522838316216777,2.44136686633116E-17));
#16705=DIRECTION('ref_axis',(0.522838316216777,-0.852431871234063,-1.10549867763274E-16));
#16706=DIRECTION('center_axis',(0.852431871234063,0.522838316216777,2.44136686633116E-17));
#16707=DIRECTION('ref_axis',(-0.522838316216777,0.852431871234063,0.));
#16708=DIRECTION('',(0.,0.,1.));
#16709=DIRECTION('',(1.,0.,0.));
#16710=DIRECTION('',(0.,0.,1.));
#16711=DIRECTION('',(1.,0.,0.));
#16712=DIRECTION('',(0.,0.,1.));
#16713=DIRECTION('',(1.,0.,0.));
#16714=DIRECTION('axis',(0.,0.,1.));
#16715=DIRECTION('refdir',(1.,0.,0.));
#16716=DIRECTION('axis',(0.,0.,1.));
#16717=DIRECTION('refdir',(1.,0.,0.));
#16718=DIRECTION('center_axis',(0.,0.,-1.));
#16719=DIRECTION('ref_axis',(-0.537828840392936,-0.843054054282162,0.));
#16720=DIRECTION('center_axis',(0.,0.,-1.));
#16721=DIRECTION('ref_axis',(0.537828840392939,0.843054054282159,0.));
#16722=DIRECTION('',(-0.38030242015954,-0.596129238689725,0.707106781186552));
#16723=DIRECTION('center_axis',(0.,0.,1.));
#16724=DIRECTION('ref_axis',(0.537828840392936,0.843054054282162,0.));
#16725=DIRECTION('center_axis',(0.,0.,1.));
#16726=DIRECTION('ref_axis',(0.53782884039294,0.843054054282159,0.));
#16727=DIRECTION('center_axis',(0.,0.,1.));
#16728=DIRECTION('ref_axis',(0.53782884039294,0.843054054282159,0.));
#16729=DIRECTION('center_axis',(0.,0.,1.));
#16730=DIRECTION('ref_axis',(0.53782884039294,0.843054054282159,0.));
#16731=DIRECTION('',(0.380302420159543,0.596129238689723,-0.707106781186552));
#16732=DIRECTION('center_axis',(0.,0.,-1.));
#16733=DIRECTION('ref_axis',(0.537828840392938,0.84305405428216,0.));
#16734=DIRECTION('center_axis',(0.,0.,-1.));
#16735=DIRECTION('ref_axis',(-0.53782884039294,-0.843054054282159,0.));
#16736=DIRECTION('',(0.,0.,1.));
#16737=DIRECTION('center_axis',(0.,0.,1.));
#16738=DIRECTION('ref_axis',(0.537828840392939,0.84305405428216,0.));
#16739=DIRECTION('center_axis',(0.,0.,1.));
#16740=DIRECTION('ref_axis',(0.537828840392939,0.84305405428216,0.));
#16741=DIRECTION('axis',(0.,0.,1.));
#16742=DIRECTION('refdir',(1.,0.,0.));
#16743=DIRECTION('center_axis',(0.,0.,1.));
#16744=DIRECTION('ref_axis',(0.916331447796931,0.400420626065117,0.));
#16745=DIRECTION('center_axis',(0.,0.,1.));
#16746=DIRECTION('ref_axis',(-0.916331447796931,-0.400420626065117,0.));
#16747=DIRECTION('center_axis',(0.,0.,1.));
#16748=DIRECTION('ref_axis',(-0.916331447796931,-0.400420626065117,0.));
#16749=DIRECTION('',(-0.647944180551693,-0.283140140017605,0.707106781186552));
#16750=DIRECTION('center_axis',(0.,0.,-1.));
#16751=DIRECTION('ref_axis',(-0.916331447796931,-0.400420626065117,0.));
#16752=DIRECTION('center_axis',(0.,0.,-1.));
#16753=DIRECTION('ref_axis',(-0.916331447796931,-0.400420626065117,0.));
#16754=DIRECTION('center_axis',(0.,0.,-1.));
#16755=DIRECTION('ref_axis',(-0.916331447796931,-0.400420626065117,0.));
#16756=DIRECTION('',(0.647944180551702,0.28314014001761,-0.707106781186541));
#16757=DIRECTION('center_axis',(0.,0.,1.));
#16758=DIRECTION('ref_axis',(-0.916331447796931,-0.400420626065117,0.));
#16759=DIRECTION('center_axis',(0.,0.,-1.));
#16760=DIRECTION('ref_axis',(-0.916331447796931,-0.400420626065117,0.));
#16761=DIRECTION('center_axis',(0.,0.,-1.));
#16762=DIRECTION('ref_axis',(-0.916331447796931,-0.400420626065116,0.));
#16763=DIRECTION('center_axis',(0.400420626065116,-0.916331447796931,0.));
#16764=DIRECTION('ref_axis',(0.916331447796931,0.400420626065116,0.));
#16765=DIRECTION('center_axis',(0.,0.,1.));
#16766=DIRECTION('ref_axis',(-0.916331447796931,-0.400420626065117,0.));
#16767=DIRECTION('center_axis',(0.,0.,1.));
#16768=DIRECTION('ref_axis',(-0.916331447796931,-0.400420626065117,0.));
#16769=DIRECTION('center_axis',(0.,0.,-1.));
#16770=DIRECTION('ref_axis',(-0.916331447796931,-0.400420626065118,0.));
#16771=DIRECTION('center_axis',(0.,0.,-1.));
#16772=DIRECTION('ref_axis',(-0.916331447796931,-0.400420626065117,0.));
#16773=DIRECTION('center_axis',(-0.400420626065117,0.916331447796931,0.));
#16774=DIRECTION('ref_axis',(0.916331447796931,0.400420626065117,0.));
#16775=DIRECTION('center_axis',(0.,0.,1.));
#16776=DIRECTION('ref_axis',(-0.916331447796931,-0.400420626065117,0.));
#16777=DIRECTION('center_axis',(0.,0.,-1.));
#16778=DIRECTION('ref_axis',(-0.916331447796931,-0.400420626065117,0.));
#16779=DIRECTION('center_axis',(0.,0.,-1.));
#16780=DIRECTION('ref_axis',(-0.916331447796931,-0.400420626065117,0.));
#16781=DIRECTION('center_axis',(0.,0.,-1.));
#16782=DIRECTION('ref_axis',(-0.916331447796931,-0.400420626065117,0.));
#16783=DIRECTION('center_axis',(0.400420626065116,-0.916331447796931,0.));
#16784=DIRECTION('ref_axis',(0.916331447796931,0.400420626065116,0.));
#16785=DIRECTION('center_axis',(0.,0.,1.));
#16786=DIRECTION('ref_axis',(-0.916331447796931,-0.400420626065116,0.));
#16787=DIRECTION('center_axis',(0.,0.,1.));
#16788=DIRECTION('ref_axis',(0.916331447796931,0.400420626065118,0.));
#16789=DIRECTION('center_axis',(0.,0.,1.));
#16790=DIRECTION('ref_axis',(0.916331447796931,0.400420626065117,0.));
#16791=DIRECTION('center_axis',(-0.400420626065117,0.916331447796931,0.));
#16792=DIRECTION('ref_axis',(-0.916331447796931,-0.400420626065117,0.));
#16793=DIRECTION('center_axis',(0.,0.,-1.));
#16794=DIRECTION('ref_axis',(0.916331447796931,0.400420626065117,0.));
#16795=DIRECTION('center_axis',(0.,0.,-1.));
#16796=DIRECTION('ref_axis',(0.916331447796931,0.400420626065117,0.));
#16797=DIRECTION('center_axis',(0.,0.,-1.));
#16798=DIRECTION('ref_axis',(-0.916331447796932,-0.400420626065115,0.));
#16799=DIRECTION('center_axis',(0.,0.,1.));
#16800=DIRECTION('ref_axis',(-0.916331447796929,-0.400420626065122,0.));
#16801=DIRECTION('',(0.,0.,-1.));
#16802=DIRECTION('center_axis',(0.,0.,-1.));
#16803=DIRECTION('ref_axis',(-0.916331447796932,-0.400420626065115,0.));
#16804=DIRECTION('center_axis',(0.,0.,1.));
#16805=DIRECTION('ref_axis',(0.916331447796932,0.400420626065116,0.));
#16806=DIRECTION('center_axis',(0.,0.,-1.));
#16807=DIRECTION('ref_axis',(-0.916331447796931,-0.400420626065116,0.));
#16808=DIRECTION('',(0.798652073797726,0.348996822238451,-0.490261239632559));
#16809=DIRECTION('center_axis',(0.,0.,-1.));
#16810=DIRECTION('ref_axis',(-0.916331447796932,-0.400420626065116,0.));
#16811=DIRECTION('center_axis',(0.,0.,-1.));
#16812=DIRECTION('ref_axis',(-0.916331447796931,-0.400420626065117,0.));
#16813=DIRECTION('',(0.,0.,-1.));
#16814=DIRECTION('center_axis',(0.,0.,-1.));
#16815=DIRECTION('ref_axis',(-0.916331447796931,-0.400420626065116,0.));
#16816=DIRECTION('center_axis',(0.,0.,-1.));
#16817=DIRECTION('ref_axis',(-0.916331447796931,-0.400420626065116,0.));
#16818=DIRECTION('',(-0.798652073797726,-0.348996822238452,0.490261239632559));
#16819=DIRECTION('center_axis',(0.,0.,-1.));
#16820=DIRECTION('ref_axis',(-0.916331447796932,-0.400420626065116,0.));
#16821=DIRECTION('center_axis',(0.,0.,-1.));
#16822=DIRECTION('ref_axis',(-0.916331447796931,-0.400420626065117,0.));
#16823=DIRECTION('',(0.,0.,-1.));
#16824=DIRECTION('center_axis',(0.,0.,1.));
#16825=DIRECTION('ref_axis',(0.916331447796931,0.400420626065116,0.));
#16826=DIRECTION('',(0.,0.,-1.));
#16827=DIRECTION('center_axis',(0.,0.,-1.));
#16828=DIRECTION('ref_axis',(-0.916331447796931,-0.400420626065117,0.));
#16829=DIRECTION('center_axis',(0.,0.,-1.));
#16830=DIRECTION('ref_axis',(-0.916331447796931,-0.400420626065117,0.));
#16831=DIRECTION('center_axis',(0.,0.,1.));
#16832=DIRECTION('ref_axis',(0.916331447796931,0.400420626065117,0.));
#16833=DIRECTION('center_axis',(0.,0.,-1.));
#16834=DIRECTION('ref_axis',(-0.916331447796931,-0.400420626065117,0.));
#16835=DIRECTION('center_axis',(0.,0.,-1.));
#16836=DIRECTION('ref_axis',(-0.916331447796931,-0.400420626065117,0.));
#16837=DIRECTION('center_axis',(0.,0.,-1.));
#16838=DIRECTION('ref_axis',(-0.916331447796931,-0.400420626065117,0.));
#16839=DIRECTION('',(0.,0.,1.));
#16840=DIRECTION('',(1.,0.,0.));
#16841=DIRECTION('',(0.,0.,1.));
#16842=DIRECTION('',(1.,0.,0.));
#16843=DIRECTION('',(0.,0.,1.));
#16844=DIRECTION('',(1.,0.,0.));
#16845=DIRECTION('axis',(0.,0.,1.));
#16846=DIRECTION('refdir',(1.,0.,0.));
#16847=DIRECTION('center_axis',(-0.223538897454057,-2.77555756156289E-16,
0.974695009387565));
#16848=DIRECTION('ref_axis',(0.945835712345015,-0.241537608024065,0.216920236867866));
#16849=DIRECTION('center_axis',(-0.223538897454057,-2.77555756156289E-16,
0.974695009387565));
#16850=DIRECTION('ref_axis',(-0.945835712345015,0.241537608024065,-0.216920236867866));
#16851=DIRECTION('center_axis',(-0.223538897454057,-2.77555756156289E-16,
0.974695009387565));
#16852=DIRECTION('ref_axis',(-0.945835712345015,0.241537608024065,-0.216920236867866));
#16853=DIRECTION('',(-0.826872716336294,0.170792880545394,0.535827680260777));
#16854=DIRECTION('center_axis',(0.223538897454057,2.77555756156289E-16,
-0.974695009387565));
#16855=DIRECTION('ref_axis',(-0.945835712345015,0.241537608024065,-0.216920236867866));
#16856=DIRECTION('center_axis',(0.223538897454057,2.77555756156289E-16,
-0.974695009387565));
#16857=DIRECTION('ref_axis',(-0.945835712345015,0.241537608024065,-0.216920236867866));
#16858=DIRECTION('center_axis',(0.223538897454057,2.77555756156289E-16,
-0.974695009387565));
#16859=DIRECTION('ref_axis',(-0.945835712345015,0.241537608024065,-0.216920236867866));
#16860=DIRECTION('',(0.826872716336301,-0.170792880545396,-0.535827680260765));
#16861=DIRECTION('center_axis',(-0.223538897454057,-2.77555756156289E-16,
0.974695009387565));
#16862=DIRECTION('ref_axis',(-0.945835712345015,0.241537608024065,-0.216920236867866));
#16863=DIRECTION('center_axis',(0.223538897454057,2.77555756156289E-16,
-0.974695009387565));
#16864=DIRECTION('ref_axis',(-0.945835712345015,0.241537608024065,-0.216920236867868));
#16865=DIRECTION('center_axis',(0.223538897454057,2.77555756156289E-16,
-0.974695009387565));
#16866=DIRECTION('ref_axis',(-0.945835712345015,0.241537608024065,-0.216920236867866));
#16867=DIRECTION('center_axis',(-0.235425501120466,-0.970391459108134,-0.0539930505913901));
#16868=DIRECTION('ref_axis',(0.945835712345015,-0.241537608024065,0.216920236867867));
#16869=DIRECTION('center_axis',(-0.223538897454057,-2.77555756156289E-16,
0.974695009387565));
#16870=DIRECTION('ref_axis',(-0.945835712345015,0.241537608024065,-0.216920236867866));
#16871=DIRECTION('center_axis',(-0.223538897454057,-2.77555756156289E-16,
0.974695009387565));
#16872=DIRECTION('ref_axis',(-0.945835712345015,0.241537608024065,-0.216920236867866));
#16873=DIRECTION('center_axis',(0.223538897454057,2.77555756156289E-16,
-0.974695009387565));
#16874=DIRECTION('ref_axis',(-0.945835712345015,0.241537608024065,-0.216920236867867));
#16875=DIRECTION('center_axis',(0.223538897454057,2.77555756156289E-16,
-0.974695009387565));
#16876=DIRECTION('ref_axis',(-0.945835712345015,0.241537608024065,-0.216920236867866));
#16877=DIRECTION('center_axis',(0.235425501120466,0.970391459108134,0.05399305059139));
#16878=DIRECTION('ref_axis',(0.945835712345015,-0.241537608024065,0.216920236867867));
#16879=DIRECTION('center_axis',(-0.223538897454057,-2.77555756156289E-16,
0.974695009387565));
#16880=DIRECTION('ref_axis',(-0.945835712345015,0.241537608024065,-0.216920236867866));
#16881=DIRECTION('center_axis',(0.223538897454057,2.77555756156289E-16,
-0.974695009387565));
#16882=DIRECTION('ref_axis',(-0.945835712345015,0.241537608024065,-0.216920236867868));
#16883=DIRECTION('center_axis',(0.223538897454057,2.77555756156289E-16,
-0.974695009387565));
#16884=DIRECTION('ref_axis',(-0.945835712345015,0.241537608024065,-0.216920236867866));
#16885=DIRECTION('center_axis',(0.223538897454057,2.77555756156289E-16,
-0.974695009387565));
#16886=DIRECTION('ref_axis',(-0.945835712345015,0.241537608024065,-0.216920236867866));
#16887=DIRECTION('center_axis',(-0.235425501120466,-0.970391459108134,-0.0539930505913901));
#16888=DIRECTION('ref_axis',(0.945835712345015,-0.241537608024065,0.216920236867867));
#16889=DIRECTION('center_axis',(-0.223538897454057,-2.77555756156289E-16,
0.974695009387565));
#16890=DIRECTION('ref_axis',(-0.945835712345015,0.241537608024065,-0.216920236867866));
#16891=DIRECTION('center_axis',(-0.223538897454057,-2.77555756156289E-16,
0.974695009387565));
#16892=DIRECTION('ref_axis',(0.945835712345015,-0.241537608024065,0.216920236867867));
#16893=DIRECTION('center_axis',(-0.223538897454057,-2.77555756156289E-16,
0.974695009387565));
#16894=DIRECTION('ref_axis',(0.945835712345015,-0.241537608024065,0.216920236867866));
#16895=DIRECTION('center_axis',(0.235425501120466,0.970391459108134,0.0539930505913899));
#16896=DIRECTION('ref_axis',(-0.945835712345015,0.241537608024065,-0.216920236867867));
#16897=DIRECTION('center_axis',(0.223538897454057,2.77555756156289E-16,
-0.974695009387565));
#16898=DIRECTION('ref_axis',(0.945835712345015,-0.241537608024065,0.216920236867866));
#16899=DIRECTION('center_axis',(0.223538897454057,2.77555756156289E-16,
-0.974695009387565));
#16900=DIRECTION('ref_axis',(0.945835712345015,-0.241537608024065,0.216920236867866));
#16901=DIRECTION('center_axis',(0.223538897454057,2.77555756156289E-16,
-0.974695009387565));
#16902=DIRECTION('ref_axis',(-0.945835712345015,0.241537608024065,-0.216920236867866));
#16903=DIRECTION('center_axis',(-0.223538897454057,-2.77555756156289E-16,
0.974695009387565));
#16904=DIRECTION('ref_axis',(-0.945835712345015,0.241537608024064,-0.216920236867866));
#16905=DIRECTION('',(0.223538897454057,2.77555756156289E-16,-0.974695009387565));
#16906=DIRECTION('center_axis',(0.223538897454057,2.77555756156289E-16,
-0.974695009387565));
#16907=DIRECTION('ref_axis',(-0.945835712345015,0.241537608024065,-0.216920236867866));
#16908=DIRECTION('center_axis',(-0.223538897454057,-2.77555756156289E-16,
0.974695009387565));
#16909=DIRECTION('ref_axis',(0.945835712345015,-0.241537608024066,0.216920236867866));
#16910=DIRECTION('center_axis',(0.223538897454057,2.77555756156289E-16,
-0.974695009387565));
#16911=DIRECTION('ref_axis',(-0.945835712345015,0.241537608024065,-0.216920236867866));
#16912=DIRECTION('',(0.933959725990609,-0.210518270449354,-0.288792811604722));
#16913=DIRECTION('center_axis',(0.223538897454057,2.77555756156289E-16,
-0.974695009387565));
#16914=DIRECTION('ref_axis',(-0.945835712345015,0.241537608024066,-0.216920236867866));
#16915=DIRECTION('center_axis',(0.223538897454057,2.77555756156289E-16,
-0.974695009387565));
#16916=DIRECTION('ref_axis',(-0.945835712345015,0.241537608024065,-0.216920236867866));
#16917=DIRECTION('',(0.223538897454057,2.77555756156289E-16,-0.974695009387564));
#16918=DIRECTION('center_axis',(0.223538897454057,2.77555756156289E-16,
-0.974695009387565));
#16919=DIRECTION('ref_axis',(-0.945835712345015,0.241537608024065,-0.216920236867866));
#16920=DIRECTION('center_axis',(0.223538897454057,2.77555756156289E-16,
-0.974695009387565));
#16921=DIRECTION('ref_axis',(-0.945835712345015,0.241537608024065,-0.216920236867866));
#16922=DIRECTION('',(-0.933959725990608,0.210518270449354,0.288792811604722));
#16923=DIRECTION('center_axis',(0.223538897454057,2.77555756156289E-16,
-0.974695009387565));
#16924=DIRECTION('ref_axis',(-0.945835712345015,0.241537608024066,-0.216920236867866));
#16925=DIRECTION('center_axis',(0.223538897454057,2.77555756156289E-16,
-0.974695009387565));
#16926=DIRECTION('ref_axis',(-0.945835712345015,0.241537608024065,-0.216920236867866));
#16927=DIRECTION('',(0.223538897454057,2.77555756156289E-16,-0.974695009387564));
#16928=DIRECTION('center_axis',(-0.223538897454057,-2.77555756156289E-16,
0.974695009387565));
#16929=DIRECTION('ref_axis',(0.945835712345015,-0.241537608024065,0.216920236867866));
#16930=DIRECTION('',(0.223538897454057,2.77555756156289E-16,-0.974695009387564));
#16931=DIRECTION('center_axis',(0.223538897454057,2.63677968348475E-16,
-0.974695009387565));
#16932=DIRECTION('ref_axis',(-0.945835712345015,0.241537608024065,-0.216920236867866));
#16933=DIRECTION('center_axis',(0.223538897454057,2.63677968348475E-16,
-0.974695009387565));
#16934=DIRECTION('ref_axis',(-0.945835712345015,0.241537608024065,-0.216920236867866));
#16935=DIRECTION('center_axis',(-0.223538897454057,-2.63677968348475E-16,
0.974695009387565));
#16936=DIRECTION('ref_axis',(0.945835712345015,-0.241537608024065,0.216920236867866));
#16937=DIRECTION('center_axis',(0.223538897454057,2.63677968348475E-16,
-0.974695009387565));
#16938=DIRECTION('ref_axis',(-0.945835712345015,0.241537608024065,-0.216920236867866));
#16939=DIRECTION('center_axis',(0.223538897454057,2.63677968348475E-16,
-0.974695009387565));
#16940=DIRECTION('ref_axis',(-0.945835712345015,0.241537608024065,-0.216920236867866));
#16941=DIRECTION('center_axis',(0.223538897454057,2.63677968348475E-16,
-0.974695009387565));
#16942=DIRECTION('ref_axis',(-0.945835712345015,0.241537608024065,-0.216920236867866));
#16943=DIRECTION('center_axis',(-0.223538897454133,0.,0.974695009387547));
#16944=DIRECTION('ref_axis',(0.974695009387547,0.,0.223538897454133));
#16945=DIRECTION('center_axis',(-0.223538897454133,0.,0.974695009387547));
#16946=DIRECTION('ref_axis',(-0.974695009387547,0.,-0.223538897454133));
#16947=DIRECTION('',(0.84727932097532,8.65956056235361E-17,-0.531147580477968));
#16948=DIRECTION('center_axis',(0.223538897454057,1.10873856701773E-16,
-0.974695009387565));
#16949=DIRECTION('ref_axis',(-0.974695009387564,4.77630626208034E-31,-0.223538897454057));
#16950=DIRECTION('center_axis',(0.223538897454062,0.,-0.974695009387563));
#16951=DIRECTION('ref_axis',(-0.974695009387563,0.,-0.223538897454062));
#16952=DIRECTION('center_axis',(0.223538897454062,0.,-0.974695009387563));
#16953=DIRECTION('ref_axis',(0.974695009387563,0.,0.223538897454062));
#16954=DIRECTION('center_axis',(0.223538897454062,0.,-0.974695009387563));
#16955=DIRECTION('ref_axis',(0.974695009387563,0.,0.223538897454062));
#16956=DIRECTION('',(-0.847279320975379,8.65956056235519E-17,0.531147580477875));
#16957=DIRECTION('center_axis',(-0.223538897454057,1.56006678063889E-16,
0.974695009387565));
#16958=DIRECTION('ref_axis',(0.974695009387565,-2.09541177949331E-31,0.223538897454057));
#16959=DIRECTION('center_axis',(-0.223538897454057,1.56006678063889E-16,
0.974695009387565));
#16960=DIRECTION('ref_axis',(0.974695009387564,6.34786509670033E-31,0.223538897454057));
#16961=DIRECTION('',(0.223538897454057,-1.56006678063889E-16,-0.974695009387564));
#16962=DIRECTION('center_axis',(0.223538897454057,1.10873856701773E-16,
-0.974695009387565));
#16963=DIRECTION('ref_axis',(-0.974695009387565,1.39180436012088E-16,-0.223538897454057));
#16964=DIRECTION('center_axis',(-0.223538897454057,1.56006678063889E-16,
0.974695009387565));
#16965=DIRECTION('ref_axis',(0.974695009387565,0.,0.223538897454057));
#16966=DIRECTION('center_axis',(0.,1.,0.));
#16967=DIRECTION('ref_axis',(0.223538897454053,0.,-0.974695009387565));
#16968=DIRECTION('',(0.,-1.,0.));
#16969=DIRECTION('',(-1.10873856701774E-16,-1.,-1.39180436012088E-16));
#16970=DIRECTION('center_axis',(0.,1.,0.));
#16971=DIRECTION('ref_axis',(0.223538897454053,0.,-0.974695009387565));
#16972=DIRECTION('',(0.,-1.,0.));
#16973=DIRECTION('center_axis',(0.,1.,0.));
#16974=DIRECTION('ref_axis',(0.223538897454053,0.,-0.974695009387565));
#16975=DIRECTION('',(0.,-1.,0.));
#16976=DIRECTION('center_axis',(0.,1.,0.));
#16977=DIRECTION('ref_axis',(0.223538897454053,0.,-0.974695009387565));
#16978=DIRECTION('',(0.,-1.,0.));
#16979=DIRECTION('center_axis',(0.,1.,0.));
#16980=DIRECTION('ref_axis',(0.223538897454053,0.,-0.974695009387565));
#16981=DIRECTION('',(0.,-1.,0.));
#16982=DIRECTION('center_axis',(0.,1.,0.));
#16983=DIRECTION('ref_axis',(0.223538897454053,0.,-0.974695009387565));
#16984=DIRECTION('',(0.,-1.,0.));
#16985=DIRECTION('center_axis',(0.,1.,0.));
#16986=DIRECTION('ref_axis',(0.223538897454053,0.,-0.974695009387565));
#16987=DIRECTION('',(0.,-1.,0.));
#16988=DIRECTION('center_axis',(0.,1.,0.));
#16989=DIRECTION('ref_axis',(0.223538897454053,0.,-0.974695009387565));
#16990=DIRECTION('',(0.,-1.,0.));
#16991=DIRECTION('center_axis',(0.,1.,0.));
#16992=DIRECTION('ref_axis',(0.223538897454053,0.,-0.974695009387565));
#16993=DIRECTION('',(0.,-1.,0.));
#16994=DIRECTION('center_axis',(0.,1.,0.));
#16995=DIRECTION('ref_axis',(0.223538897454053,0.,-0.974695009387565));
#16996=DIRECTION('',(0.,-1.,0.));
#16997=DIRECTION('center_axis',(0.,1.,0.));
#16998=DIRECTION('ref_axis',(0.223538897454053,0.,-0.974695009387565));
#16999=DIRECTION('',(0.,-1.,0.));
#17000=DIRECTION('center_axis',(0.,1.,0.));
#17001=DIRECTION('ref_axis',(0.223538897454053,0.,-0.974695009387565));
#17002=DIRECTION('',(0.,-1.,0.));
#17003=DIRECTION('center_axis',(0.,1.,0.));
#17004=DIRECTION('ref_axis',(0.223538897454053,0.,-0.974695009387565));
#17005=DIRECTION('',(0.,-1.,0.));
#17006=DIRECTION('center_axis',(4.06756404254584E-31,1.,1.13752359080447E-16));
#17007=DIRECTION('ref_axis',(-0.974695009387565,2.54280769316413E-17,-0.223538897454056));
#17008=DIRECTION('',(-4.06756404254584E-31,-1.,-1.13752359080446E-16));
#17009=DIRECTION('',(-4.06756404254584E-31,-1.,-1.13752359080446E-16));
#17010=DIRECTION('center_axis',(4.06756404254584E-31,1.,1.13752359080447E-16));
#17011=DIRECTION('ref_axis',(-0.974695009387565,2.54280769316413E-17,-0.223538897454056));
#17012=DIRECTION('',(1.10873856701774E-16,1.,1.39180436012088E-16));
#17013=DIRECTION('center_axis',(4.06756404254584E-31,1.,1.13752359080447E-16));
#17014=DIRECTION('ref_axis',(-0.974695009387565,2.54280769316413E-17,-0.223538897454056));
#17015=DIRECTION('',(-4.06756404254584E-31,-1.,-1.13752359080446E-16));
#17016=DIRECTION('center_axis',(4.06756404254584E-31,1.,1.13752359080447E-16));
#17017=DIRECTION('ref_axis',(-0.974695009387565,2.54280769316413E-17,-0.223538897454056));
#17018=DIRECTION('',(-4.06756404254584E-31,-1.,-1.13752359080446E-16));
#17019=DIRECTION('center_axis',(4.06756404254584E-31,1.,1.13752359080447E-16));
#17020=DIRECTION('ref_axis',(-0.974695009387565,2.54280769316413E-17,-0.223538897454056));
#17021=DIRECTION('',(-4.06756404254584E-31,-1.,-1.13752359080446E-16));
#17022=DIRECTION('center_axis',(4.06756404254584E-31,1.,1.13752359080447E-16));
#17023=DIRECTION('ref_axis',(-0.974695009387565,2.54280769316413E-17,-0.223538897454056));
#17024=DIRECTION('',(-4.06756404254584E-31,-1.,-1.13752359080446E-16));
#17025=DIRECTION('center_axis',(4.06756404254584E-31,1.,1.13752359080447E-16));
#17026=DIRECTION('ref_axis',(-0.974695009387565,2.54280769316413E-17,-0.223538897454056));
#17027=DIRECTION('',(-4.06756404254584E-31,-1.,-1.13752359080446E-16));
#17028=DIRECTION('center_axis',(4.06756404254584E-31,1.,1.13752359080447E-16));
#17029=DIRECTION('ref_axis',(-0.974695009387565,2.54280769316413E-17,-0.223538897454056));
#17030=DIRECTION('',(-4.06756404254584E-31,-1.,-1.13752359080446E-16));
#17031=DIRECTION('center_axis',(4.06756404254584E-31,1.,1.13752359080447E-16));
#17032=DIRECTION('ref_axis',(-0.974695009387565,2.54280769316413E-17,-0.223538897454056));
#17033=DIRECTION('',(-4.06756404254584E-31,-1.,-1.13752359080446E-16));
#17034=DIRECTION('center_axis',(4.06756404254584E-31,1.,1.13752359080447E-16));
#17035=DIRECTION('ref_axis',(-0.974695009387565,2.54280769316413E-17,-0.223538897454056));
#17036=DIRECTION('',(-4.06756404254584E-31,-1.,-1.13752359080446E-16));
#17037=DIRECTION('center_axis',(4.06756404254584E-31,1.,1.13752359080447E-16));
#17038=DIRECTION('ref_axis',(-0.974695009387565,2.54280769316413E-17,-0.223538897454056));
#17039=DIRECTION('',(-4.06756404254584E-31,-1.,-1.13752359080446E-16));
#17040=DIRECTION('center_axis',(4.06756404254584E-31,1.,1.13752359080447E-16));
#17041=DIRECTION('ref_axis',(-0.974695009387565,2.54280769316413E-17,-0.223538897454056));
#17042=DIRECTION('',(-4.06756404254584E-31,-1.,-1.13752359080446E-16));
#17043=DIRECTION('center_axis',(4.06756404254584E-31,1.,1.13752359080447E-16));
#17044=DIRECTION('ref_axis',(-0.974695009387565,2.54280769316413E-17,-0.223538897454056));
#17045=DIRECTION('',(-4.06756404254584E-31,-1.,-1.13752359080446E-16));
#17046=DIRECTION('center_axis',(4.06756404254584E-31,1.,1.13752359080447E-16));
#17047=DIRECTION('ref_axis',(-0.974695009387565,2.54280769316413E-17,-0.223538897454056));
#17048=DIRECTION('center_axis',(-1.10873856701774E-16,-1.,-1.39180436012088E-16));
#17049=DIRECTION('ref_axis',(-0.974695009387565,1.39180436012088E-16,-0.223538897454056));
#17050=DIRECTION('center_axis',(4.06756404254584E-31,1.,1.13752359080447E-16));
#17051=DIRECTION('ref_axis',(-0.974695009387565,2.54280769316414E-17,-0.223538897454057));
#17052=DIRECTION('center_axis',(4.06756404254584E-31,1.,1.13752359080447E-16));
#17053=DIRECTION('ref_axis',(-0.974695009387565,2.54280769316414E-17,-0.223538897454057));
#17054=DIRECTION('',(-4.06756404254584E-31,-1.,-1.13752359080447E-16));
#17055=DIRECTION('center_axis',(4.06756404254584E-31,1.,1.13752359080447E-16));
#17056=DIRECTION('ref_axis',(-0.974695009387565,2.54280769316413E-17,-0.223538897454056));
#17057=DIRECTION('center_axis',(4.06756404254584E-31,1.,1.13752359080447E-16));
#17058=DIRECTION('ref_axis',(-0.974695009387565,2.54280769316413E-17,-0.223538897454056));
#17059=DIRECTION('center_axis',(4.06756404254584E-31,1.,1.13752359080447E-16));
#17060=DIRECTION('ref_axis',(-0.974695009387565,2.54280769316413E-17,-0.223538897454056));
#17061=DIRECTION('center_axis',(4.06756404254584E-31,1.,1.13752359080447E-16));
#17062=DIRECTION('ref_axis',(-0.974695009387565,2.54280769316413E-17,-0.223538897454056));
#17063=DIRECTION('center_axis',(-0.223538897454057,1.56006678063889E-16,
0.974695009387565));
#17064=DIRECTION('ref_axis',(3.48735608098719E-17,1.,-1.52058930540005E-16));
#17065=DIRECTION('center_axis',(0.223538897454057,-8.18731961845386E-17,
-0.974695009387565));
#17066=DIRECTION('ref_axis',(-1.83018440061315E-17,-1.,7.98013957236788E-17));
#17067=DIRECTION('',(-0.223538897454057,1.56006678063889E-16,0.974695009387564));
#17068=DIRECTION('center_axis',(-0.223538897454057,1.56006678063889E-16,
0.974695009387565));
#17069=DIRECTION('ref_axis',(3.48735608098719E-17,1.,-1.52058930540005E-16));
#17070=DIRECTION('center_axis',(-0.223538897454057,1.56006678063889E-16,
0.974695009387565));
#17071=DIRECTION('ref_axis',(3.48735608098719E-17,1.,-1.52058930540005E-16));
#17072=DIRECTION('center_axis',(-0.223538897454057,1.56006678063889E-16,
0.974695009387565));
#17073=DIRECTION('ref_axis',(3.48735608098719E-17,1.,-1.52058930540005E-16));
#17074=DIRECTION('',(-0.223538897454057,1.56006678063889E-16,0.974695009387564));
#17075=DIRECTION('center_axis',(-0.223538897454057,-1.45003302586173E-17,
0.974695009387565));
#17076=DIRECTION('ref_axis',(-3.24138783873102E-18,1.,1.41333995375458E-17));
#17077=DIRECTION('center_axis',(-1.10873856701774E-16,-1.,-1.39180436012088E-16));
#17078=DIRECTION('ref_axis',(0.974695009387565,-1.39180436012088E-16,0.223538897454055));
#17079=DIRECTION('',(0.689213450726628,0.707106781186552,0.158065870248726));
#17080=DIRECTION('center_axis',(4.06756404254584E-31,1.,1.13752359080447E-16));
#17081=DIRECTION('ref_axis',(-0.974695009387565,2.54280769316412E-17,-0.223538897454055));
#17082=DIRECTION('center_axis',(9.65226914079907E-15,1.,-2.54344969793374E-14));
#17083=DIRECTION('ref_axis',(-0.41021732252356,-1.99199681972541E-14,-0.911987800522354));
#17084=DIRECTION('center_axis',(1.62577613129444E-16,1.,-8.62630726148516E-17));
#17085=DIRECTION('ref_axis',(0.223538897454057,-1.20422606761801E-16,-0.974695009387565));
#17086=DIRECTION('',(0.223538897454057,-1.20422606761801E-16,-0.974695009387564));
#17087=DIRECTION('',(-0.974695009387564,1.39180436012088E-16,-0.223538897454057));
#17088=DIRECTION('',(0.974695009387564,-1.39180436012088E-16,0.223538897454057));
#17089=DIRECTION('center_axis',(1.62577613129444E-16,1.,-8.62630726148516E-17));
#17090=DIRECTION('ref_axis',(0.223538897454057,-1.20422606761801E-16,-0.974695009387565));
#17091=DIRECTION('',(0.223538897454057,-1.20422606761801E-16,-0.974695009387564));
#17092=DIRECTION('',(0.974695009387564,-1.39180436012088E-16,0.223538897454057));
#17093=DIRECTION('center_axis',(-0.223538897454057,-1.45003302586173E-17,
0.974695009387565));
#17094=DIRECTION('ref_axis',(1.32417088546636E-16,1.,4.52456407508629E-17));
#17095=DIRECTION('',(-0.0358554746668518,-0.999323153056184,-0.00822318078734816));
#17096=DIRECTION('',(-0.974695009387564,1.39180436012088E-16,-0.223538897454057));
#17097=DIRECTION('',(-0.34917785007855,0.933628307384311,-0.0800812878594524));
#17098=DIRECTION('center_axis',(0.223538897454057,1.45003302586173E-17,
-0.974695009387565));
#17099=DIRECTION('ref_axis',(-3.24138783873102E-18,1.,1.41333995375458E-17));
#17100=DIRECTION('center_axis',(0.223538897454057,1.10873856701773E-16,
-0.974695009387565));
#17101=DIRECTION('ref_axis',(-0.974695009387565,1.39180436012088E-16,-0.223538897454057));
#17102=DIRECTION('',(-0.34917785007855,0.933628307384311,-0.0800812878594525));
#17103=DIRECTION('',(0.974695009387564,-1.39180436012088E-16,0.223538897454057));
#17104=DIRECTION('',(-0.0358554746668519,-0.999323153056184,-0.00822318078734794));
#17105=DIRECTION('center_axis',(0.223538897454057,-1.56006678063889E-16,
-0.974695009387565));
#17106=DIRECTION('ref_axis',(-3.48735608098719E-17,-1.,1.52058930540005E-16));
#17107=DIRECTION('center_axis',(1.62577613129444E-16,1.,-8.62630726148516E-17));
#17108=DIRECTION('ref_axis',(0.223538897454057,-1.20422606761801E-16,-0.974695009387565));
#17109=DIRECTION('',(-0.974695009387565,1.39180436012088E-16,-0.223538897454057));
#17110=DIRECTION('',(0.223538897454057,-1.20422606761801E-16,-0.974695009387564));
#17111=DIRECTION('center_axis',(-0.223538897454057,1.56006678063889E-16,
0.974695009387565));
#17112=DIRECTION('ref_axis',(1.70532037195239E-16,1.,-1.20946689326688E-16));
#17113=DIRECTION('',(-0.0358554746668519,-0.999323153056184,-0.00822318078734794));
#17114=DIRECTION('',(-0.974695009387564,1.39180436012088E-16,-0.223538897454057));
#17115=DIRECTION('',(-0.34917785007855,0.933628307384311,-0.0800812878594525));
#17116=DIRECTION('center_axis',(0.223538897454057,-1.56006678063889E-16,
-0.974695009387565));
#17117=DIRECTION('ref_axis',(-3.48735608098719E-17,-1.,1.52058930540005E-16));
#17118=DIRECTION('center_axis',(0.223538897454057,-8.18731961845386E-17,
-0.974695009387565));
#17119=DIRECTION('ref_axis',(-1.53960320391499E-16,-1.,4.86891545103617E-17));
#17120=DIRECTION('',(0.34917785007855,-0.933628307384311,0.0800812878594524));
#17121=DIRECTION('',(0.974695009387564,-1.39180436012088E-16,0.223538897454057));
#17122=DIRECTION('',(0.0358554746668518,0.999323153056184,0.00822318078734806));
#17123=DIRECTION('center_axis',(-0.223538897454057,8.18731961845386E-17,
0.974695009387565));
#17124=DIRECTION('ref_axis',(-1.83018440061315E-17,-1.,7.98013957236788E-17));
#17125=DIRECTION('center_axis',(-1.10873856701774E-16,-1.,-1.39180436012088E-16));
#17126=DIRECTION('ref_axis',(0.974695009387565,-1.39180436012088E-16,0.223538897454057));
#17127=DIRECTION('',(-0.223538897454057,-1.10873856701773E-16,0.974695009387564));
#17128=DIRECTION('',(-0.974695009387564,1.39180436012088E-16,-0.223538897454057));
#17129=DIRECTION('',(-0.223538897454057,-1.10873856701773E-16,0.974695009387564));
#17130=DIRECTION('',(0.974695009387564,-1.39180436012088E-16,0.223538897454057));
#17131=DIRECTION('center_axis',(0.974695009387565,-1.39180436012088E-16,
0.223538897454057));
#17132=DIRECTION('ref_axis',(0.223538897454057,1.10873856701773E-16,-0.974695009387565));
#17133=DIRECTION('',(-0.223538897454057,1.56006678063889E-16,0.974695009387564));
#17134=DIRECTION('center_axis',(0.974695009387565,-1.39180436012088E-16,
0.223538897454057));
#17135=DIRECTION('ref_axis',(0.223538897454057,6.16297582203915E-33,-0.974695009387565));
#17136=DIRECTION('center_axis',(0.974695009387565,-1.39180436012088E-16,
0.223538897454057));
#17137=DIRECTION('ref_axis',(0.223538897454057,6.16297582203915E-33,-0.974695009387565));
#17138=DIRECTION('',(-0.223538897454057,1.56006678063889E-16,0.974695009387564));
#17139=DIRECTION('center_axis',(0.974695009387565,-1.39180436012088E-16,
0.223538897454057));
#17140=DIRECTION('ref_axis',(0.223538897454057,1.10873856701773E-16,-0.974695009387565));
#17141=DIRECTION('center_axis',(-0.974695009387565,1.39180436012088E-16,
-0.223538897454057));
#17142=DIRECTION('ref_axis',(0.223538897454057,5.55111512312581E-15,-0.974695009387565));
#17143=DIRECTION('',(-0.223538897454057,1.56006678063889E-16,0.974695009387564));
#17144=DIRECTION('',(-0.223538897454057,1.56006678063889E-16,0.974695009387564));
#17145=DIRECTION('center_axis',(-0.974695009387565,1.39180436012088E-16,
-0.223538897454057));
#17146=DIRECTION('ref_axis',(0.223538897454057,6.16297582203915E-33,-0.974695009387565));
#17147=DIRECTION('center_axis',(0.910002851830447,0.358243190655045,0.208702242464586));
#17148=DIRECTION('ref_axis',(-0.34917785007855,0.933628307384311,-0.0800812878594523));
#17149=DIRECTION('center_axis',(-0.910002851830524,-0.358243190654995,-0.208702242464336));
#17150=DIRECTION('ref_axis',(0.349177850069457,-0.93362830738433,0.0800812878988744));
#17151=DIRECTION('center_axis',(0.910002851830446,0.358243190655048,0.208702242464584));
#17152=DIRECTION('ref_axis',(0.349177850078086,-0.93362830738431,0.0800812878614929));
#17153=DIRECTION('',(-0.223538897454057,1.56006678063889E-16,0.974695009387564));
#17154=DIRECTION('center_axis',(-0.974035290049308,0.0367863529837719,-0.223387595834492));
#17155=DIRECTION('ref_axis',(-0.0358554746668518,-0.999323153056184,-0.00822318078734825));
#17156=DIRECTION('center_axis',(0.974035290049308,-0.0367863529837719,0.223387595834492));
#17157=DIRECTION('ref_axis',(0.0358554746668518,0.999323153056184,0.00822318078734814));
#17158=DIRECTION('',(-0.223538897454057,1.56006678063889E-16,0.974695009387564));
#17159=DIRECTION('center_axis',(-0.974035290049323,0.0367863529838382,-0.223387595834417));
#17160=DIRECTION('ref_axis',(0.0358554746968573,0.999323153056181,0.00822318065681202));
#17161=DIRECTION('center_axis',(-0.223538897454057,1.56006678063889E-16,
0.974695009387565));
#17162=DIRECTION('ref_axis',(0.159899237082201,-0.986451936077797,0.0366716755670673));
#17163=DIRECTION('center_axis',(-0.223538897454057,1.56006678063889E-16,
0.974695009387565));
#17164=DIRECTION('ref_axis',(0.159899237082201,-0.986451936077797,0.0366716755670673));
#17165=DIRECTION('',(-0.223538897454057,1.56006678063889E-16,0.974695009387565));
#17166=DIRECTION('',(-0.223538897454057,1.56006678063889E-16,0.974695009387564));
#17167=DIRECTION('center_axis',(-0.974035290049308,0.0367863529837719,-0.223387595834492));
#17168=DIRECTION('ref_axis',(-0.0358554746668518,-0.999323153056184,-0.00822318078734825));
#17169=DIRECTION('center_axis',(0.974035290049308,-0.0367863529837719,0.223387595834492));
#17170=DIRECTION('ref_axis',(0.0358554746668518,0.999323153056184,0.00822318078734814));
#17171=DIRECTION('center_axis',(-0.974035290049297,0.0367863529838035,-0.223387595834534));
#17172=DIRECTION('ref_axis',(0.0358554743858934,0.999323153056183,0.00822318201255029));
#17173=DIRECTION('center_axis',(0.910002851830447,0.358243190655045,0.208702242464586));
#17174=DIRECTION('ref_axis',(-0.34917785007855,0.933628307384311,-0.0800812878594523));
#17175=DIRECTION('center_axis',(-0.910002851830389,-0.358243190654987,-0.208702242464939));
#17176=DIRECTION('ref_axis',(0.349177850195129,-0.933628307384333,0.080081287350873));
#17177=DIRECTION('center_axis',(0.910002851830444,0.358243190655049,0.20870224246459));
#17178=DIRECTION('ref_axis',(0.349177850076088,-0.933628307384309,0.0800812878702079));
#17179=DIRECTION('center_axis',(4.19082355898663E-31,1.,1.13752359080447E-16));
#17180=DIRECTION('ref_axis',(-0.974695009387565,2.54280769316415E-17,-0.223538897454057));
#17181=DIRECTION('center_axis',(4.19082355898663E-31,1.,1.13752359080447E-16));
#17182=DIRECTION('ref_axis',(-0.974695009387565,2.54280769316415E-17,-0.223538897454057));
#17183=DIRECTION('center_axis',(0.974695009387565,-1.39180436012088E-16,
0.223538897454057));
#17184=DIRECTION('ref_axis',(0.223538897454057,1.10873856701773E-16,-0.974695009387565));
#17185=DIRECTION('',(-0.193590363929179,-0.499999999999996,0.844110639071545));
#17186=DIRECTION('',(0.193590363929179,-0.499999999999996,-0.844110639071545));
#17187=DIRECTION('center_axis',(0.,1.,0.));
#17188=DIRECTION('ref_axis',(0.223538897454053,0.,-0.974695009387565));
#17189=DIRECTION('center_axis',(-0.974695009387565,1.39180436012088E-16,
-0.223538897454057));
#17190=DIRECTION('ref_axis',(-0.223538897454057,-6.16297582203915E-33,0.974695009387565));
#17191=DIRECTION('center_axis',(-0.974695009387565,1.39180436012088E-16,
-0.223538897454057));
#17192=DIRECTION('ref_axis',(-0.223538897454057,-6.16297582203915E-33,0.974695009387565));
#17193=DIRECTION('center_axis',(0.974695009387565,-1.39180436012088E-16,
0.223538897454057));
#17194=DIRECTION('ref_axis',(0.223538897454057,-1.10317267214501E-30,-0.974695009387565));
#17195=DIRECTION('center_axis',(0.974695009387565,-1.39180436012088E-16,
0.223538897454057));
#17196=DIRECTION('ref_axis',(0.223538897454057,-1.10317267214501E-30,-0.974695009387565));
#17197=DIRECTION('center_axis',(0.,-1.,0.));
#17198=DIRECTION('ref_axis',(-0.99646141012762,0.,-0.0840515206672309));
#17199=DIRECTION('',(0.,1.,0.));
#17200=DIRECTION('center_axis',(-4.15314294130208E-14,-1.,-7.5151094970912E-14));
#17201=DIRECTION('ref_axis',(0.303675785059601,-8.33478827153308E-14,0.952775428717825));
#17202=DIRECTION('center_axis',(0.,-1.,0.));
#17203=DIRECTION('ref_axis',(-0.99646141012762,0.,-0.0840515206672309));
#17204=DIRECTION('',(0.,1.,0.));
#17205=DIRECTION('center_axis',(0.,-1.,0.));
#17206=DIRECTION('ref_axis',(-0.99646141012762,0.,-0.0840515206672309));
#17207=DIRECTION('',(0.,1.,0.));
#17208=DIRECTION('center_axis',(0.,-1.,0.));
#17209=DIRECTION('ref_axis',(-0.99646141012762,0.,-0.0840515206672309));
#17210=DIRECTION('',(0.,1.,0.));
#17211=DIRECTION('center_axis',(0.,-1.,0.));
#17212=DIRECTION('ref_axis',(-0.99646141012762,0.,-0.0840515206672309));
#17213=DIRECTION('',(0.,1.,0.));
#17214=DIRECTION('center_axis',(0.,-1.,0.));
#17215=DIRECTION('ref_axis',(-0.99646141012762,0.,-0.0840515206672309));
#17216=DIRECTION('',(0.,1.,0.));
#17217=DIRECTION('center_axis',(0.,-1.,0.));
#17218=DIRECTION('ref_axis',(-0.99646141012762,0.,-0.0840515206672309));
#17219=DIRECTION('',(0.,1.,0.));
#17220=DIRECTION('center_axis',(0.,-1.,0.));
#17221=DIRECTION('ref_axis',(-0.99646141012762,0.,-0.0840515206672309));
#17222=DIRECTION('',(0.,1.,0.));
#17223=DIRECTION('',(4.52978722919878E-31,1.,1.13752359080446E-16));
#17224=DIRECTION('center_axis',(-4.52978722919878E-31,-1.,-1.13752359080446E-16));
#17225=DIRECTION('ref_axis',(-0.99646141012762,9.56105876019769E-18,-0.0840515206672388));
#17226=DIRECTION('',(-4.52978722919878E-31,-1.,-1.13752359080446E-16));
#17227=DIRECTION('',(-4.52978722919878E-31,-1.,-1.13752359080446E-16));
#17228=DIRECTION('',(-4.52978722919878E-31,-1.,-1.13752359080446E-16));
#17229=DIRECTION('center_axis',(4.52978722919878E-31,1.,1.13752359080446E-16));
#17230=DIRECTION('ref_axis',(0.99646141012762,-9.56105876019769E-18,0.0840515206672388));
#17231=DIRECTION('center_axis',(-4.52978722919878E-31,-1.,-1.13752359080446E-16));
#17232=DIRECTION('ref_axis',(-0.99646141012762,9.56105876019769E-18,-0.0840515206672388));
#17233=DIRECTION('',(-4.52978722919878E-31,-1.,-1.13752359080446E-16));
#17234=DIRECTION('center_axis',(-4.52978722919878E-31,-1.,-1.13752359080446E-16));
#17235=DIRECTION('ref_axis',(-0.99646141012762,9.56105876019769E-18,-0.0840515206672388));
#17236=DIRECTION('',(-4.52978722919878E-31,-1.,-1.13752359080446E-16));
#17237=DIRECTION('center_axis',(-4.52978722919878E-31,-1.,-1.13752359080446E-16));
#17238=DIRECTION('ref_axis',(-0.99646141012762,9.56105876019769E-18,-0.0840515206672388));
#17239=DIRECTION('',(-4.52978722919878E-31,-1.,-1.13752359080446E-16));
#17240=DIRECTION('center_axis',(-4.52978722919878E-31,-1.,-1.13752359080446E-16));
#17241=DIRECTION('ref_axis',(-0.99646141012762,9.56105876019769E-18,-0.0840515206672388));
#17242=DIRECTION('',(-4.52978722919878E-31,-1.,-1.13752359080446E-16));
#17243=DIRECTION('center_axis',(-4.52978722919878E-31,-1.,-1.13752359080446E-16));
#17244=DIRECTION('ref_axis',(-0.99646141012762,9.56105876019769E-18,-0.0840515206672388));
#17245=DIRECTION('',(-4.52978722919878E-31,-1.,-1.13752359080446E-16));
#17246=DIRECTION('center_axis',(-4.52978722919878E-31,-1.,-1.13752359080446E-16));
#17247=DIRECTION('ref_axis',(-0.99646141012762,9.56105876019769E-18,-0.0840515206672388));
#17248=DIRECTION('',(-4.52978722919878E-31,-1.,-1.13752359080446E-16));
#17249=DIRECTION('center_axis',(-4.52978722919878E-31,-1.,-1.13752359080446E-16));
#17250=DIRECTION('ref_axis',(-0.99646141012762,9.56105876019769E-18,-0.0840515206672388));
#17251=DIRECTION('',(-4.52978722919878E-31,-1.,-1.13752359080446E-16));
#17252=DIRECTION('center_axis',(4.52978722919878E-31,1.,1.13752359080446E-16));
#17253=DIRECTION('ref_axis',(0.99646141012762,-9.56105876019769E-18,0.0840515206672388));
#17254=DIRECTION('center_axis',(-4.52978722919878E-31,-1.,-1.13752359080446E-16));
#17255=DIRECTION('ref_axis',(-0.99646141012762,9.56105876019769E-18,-0.0840515206672388));
#17256=DIRECTION('center_axis',(-4.52978722919878E-31,-1.,-1.13752359080446E-16));
#17257=DIRECTION('ref_axis',(-0.99646141012762,9.56105876019769E-18,-0.0840515206672388));
#17258=DIRECTION('center_axis',(4.52978722919878E-31,1.,1.13752359080446E-16));
#17259=DIRECTION('ref_axis',(0.99646141012762,-9.56105876019769E-18,0.0840515206672388));
#17260=DIRECTION('',(4.52978722919878E-31,1.,1.13752359080446E-16));
#17261=DIRECTION('center_axis',(4.52978722919878E-31,1.,1.13752359080446E-16));
#17262=DIRECTION('ref_axis',(0.99646141012762,-9.56105876019769E-18,0.0840515206672388));
#17263=DIRECTION('center_axis',(4.51437978964368E-31,1.,1.13752359080446E-16));
#17264=DIRECTION('ref_axis',(0.99646141012762,-9.56105876019768E-18,0.0840515206672388));
#17265=DIRECTION('',(0.99646141012762,-9.56105876019769E-18,0.0840515206672387));
#17266=DIRECTION('',(0.904986655395003,4.83947982939151E-17,-0.425439952939268));
#17267=DIRECTION('',(0.571021457188351,9.33833082273063E-17,-0.820935134727764));
#17268=DIRECTION('',(0.0840515206672388,1.13349836134644E-16,-0.99646141012762));
#17269=DIRECTION('',(-0.425439952939269,1.02944366987504E-16,-0.904986655395002));
#17270=DIRECTION('',(-0.820935134727764,6.4955037840729E-17,-0.571021457188351));
#17271=DIRECTION('',(-0.99646141012762,9.56105876019769E-18,-0.0840515206672387));
#17272=DIRECTION('',(-0.904986655395003,-4.83947982939151E-17,0.425439952939268));
#17273=DIRECTION('',(-0.571021457188351,-9.33833082273063E-17,0.820935134727764));
#17274=DIRECTION('',(-0.0840515206672388,-1.13349836134644E-16,0.99646141012762));
#17275=DIRECTION('',(0.425439952939269,-1.02944366987504E-16,0.904986655395002));
#17276=DIRECTION('',(0.820935134727764,-6.4955037840729E-17,0.571021457188351));
#17277=DIRECTION('center_axis',(4.51437978964368E-31,1.,1.13752359080446E-16));
#17278=DIRECTION('ref_axis',(0.99646141012762,-9.56105876019768E-18,0.0840515206672388));
#17279=DIRECTION('',(0.99646141012762,-9.56105876019769E-18,0.0840515206672387));
#17280=DIRECTION('',(0.425439952939269,-1.02944366987504E-16,0.904986655395002));
#17281=DIRECTION('',(-0.571021457188351,-9.33833082273063E-17,0.820935134727764));
#17282=DIRECTION('',(-0.99646141012762,9.56105876019769E-18,-0.0840515206672387));
#17283=DIRECTION('',(-0.425439952939269,1.02944366987504E-16,-0.904986655395002));
#17284=DIRECTION('',(0.571021457188351,9.33833082273063E-17,-0.820935134727764));
#17285=DIRECTION('center_axis',(4.51437978964368E-31,1.,1.13752359080446E-16));
#17286=DIRECTION('ref_axis',(0.99646141012762,-9.56105876019768E-18,0.0840515206672388));
#17287=DIRECTION('center_axis',(0.0840515206672388,1.13349836134644E-16,
-0.99646141012762));
#17288=DIRECTION('ref_axis',(4.54519466875388E-31,1.,1.13752359080446E-16));
#17289=DIRECTION('',(0.70460462029195,-0.707106781186548,0.0594334002328457));
#17290=DIRECTION('',(0.704604620291949,0.707106781186547,0.0594334002328458));
#17291=DIRECTION('',(-4.52978722919878E-31,-1.,-1.13752359080446E-16));
#17292=DIRECTION('',(-4.52978722919878E-31,-1.,-1.13752359080446E-16));
#17293=DIRECTION('center_axis',(-0.820935134727764,6.4955037840729E-17,
-0.571021457188352));
#17294=DIRECTION('ref_axis',(-0.571021457188352,-9.33833082273063E-17,0.820935134727764));
#17295=DIRECTION('',(0.403773144580907,0.707106781186548,-0.580488800680294));
#17296=DIRECTION('',(-4.52978722919878E-31,-1.,-1.13752359080446E-16));
#17297=DIRECTION('',(0.403773144580907,-0.707106781186547,-0.580488800680294));
#17298=DIRECTION('center_axis',(-0.904986655395002,-4.83947982939152E-17,
0.425439952939269));
#17299=DIRECTION('ref_axis',(0.425439952939269,-1.02944366987504E-16,0.904986655395002));
#17300=DIRECTION('',(-0.300831475711043,-0.707106781186547,-0.63992220091314));
#17301=DIRECTION('',(-0.300831475711043,0.707106781186548,-0.639922200913139));
#17302=DIRECTION('',(-4.52978722919878E-31,-1.,-1.13752359080446E-16));
#17303=DIRECTION('center_axis',(-0.0840515206672388,-1.13349836134644E-16,
0.99646141012762));
#17304=DIRECTION('ref_axis',(-4.54519466875388E-31,-1.,-1.13752359080446E-16));
#17305=DIRECTION('',(-0.70460462029195,0.707106781186548,-0.0594334002328457));
#17306=DIRECTION('',(-4.52978722919878E-31,-1.,-1.13752359080446E-16));
#17307=DIRECTION('',(-0.704604620291949,-0.707106781186547,-0.0594334002328458));
#17308=DIRECTION('center_axis',(0.820935134727764,-6.4955037840729E-17,
0.571021457188352));
#17309=DIRECTION('ref_axis',(0.571021457188352,9.33833082273063E-17,-0.820935134727764));
#17310=DIRECTION('',(-0.403773144580907,-0.707106781186548,0.580488800680294));
#17311=DIRECTION('',(-0.403773144580907,0.707106781186547,0.580488800680294));
#17312=DIRECTION('',(-4.52978722919878E-31,-1.,-1.13752359080446E-16));
#17313=DIRECTION('center_axis',(0.904986655395002,4.83947982939152E-17,
-0.425439952939269));
#17314=DIRECTION('ref_axis',(-0.425439952939269,1.02944366987504E-16,-0.904986655395002));
#17315=DIRECTION('',(0.300831475711043,-0.707106781186548,0.639922200913139));
#17316=DIRECTION('',(0.300831475711043,0.707106781186548,0.639922200913139));
#17317=DIRECTION('center_axis',(0.0840515206672388,1.13349836134644E-16,
-0.99646141012762));
#17318=DIRECTION('ref_axis',(4.54519466875388E-31,1.,1.13752359080446E-16));
#17319=DIRECTION('',(-0.862960895061384,0.499999999999998,-0.0727907521245416));
#17320=DIRECTION('',(0.862960895061384,0.499999999999998,0.0727907521245417));
#17321=DIRECTION('center_axis',(0.,-1.,0.));
#17322=DIRECTION('ref_axis',(-0.99646141012762,0.,-0.0840515206672309));
#17323=DIRECTION('center_axis',(-0.380525062046606,0.447213595499958,-0.809444672077361));
#17324=DIRECTION('ref_axis',(-0.0420257603336194,0.866025403784439,0.49823070506381));
#17325=DIRECTION('center_axis',(0.891262180000262,0.447213595499958,0.0751779655296698));
#17326=DIRECTION('ref_axis',(0.445631090000131,-0.894427190999916,0.0375889827648348));
#17327=DIRECTION('center_axis',(0.510737117953656,0.447213595499958,-0.734266706547691));
#17328=DIRECTION('ref_axis',(-0.0420257603336193,0.866025403784439,0.49823070506381));
#17329=DIRECTION('center_axis',(-0.891262180000262,0.447213595499958,-0.0751779655296697));
#17330=DIRECTION('ref_axis',(0.445631090000131,0.894427190999916,0.037588982764835));
#17331=DIRECTION('center_axis',(-0.510737117953656,0.447213595499958,0.734266706547692));
#17332=DIRECTION('ref_axis',(-0.0420257603336193,-0.866025403784439,0.49823070506381));
#17333=DIRECTION('center_axis',(0.380525062046606,0.447213595499958,0.809444672077361));
#17334=DIRECTION('ref_axis',(-0.0420257603336194,-0.866025403784439,0.49823070506381));
#17335=DIRECTION('axis',(0.,0.,1.));
#17336=DIRECTION('refdir',(1.,0.,0.));
#17337=DIRECTION('center_axis',(0.,0.,1.));
#17338=DIRECTION('ref_axis',(0.893719561472763,-0.448626064156924,0.));
#17339=DIRECTION('center_axis',(0.,0.,1.));
#17340=DIRECTION('ref_axis',(-0.893719561472763,0.448626064156923,0.));
#17341=DIRECTION('',(0.631955162396449,-0.317226532182388,-0.707106781186558));
#17342=DIRECTION('center_axis',(0.,0.,-1.));
#17343=DIRECTION('ref_axis',(-0.893719561472763,0.448626064156925,0.));
#17344=DIRECTION('center_axis',(0.,0.,-1.));
#17345=DIRECTION('ref_axis',(-0.893719561472763,0.448626064156923,0.));
#17346=DIRECTION('center_axis',(0.,0.,-1.));
#17347=DIRECTION('ref_axis',(-0.893719561472763,0.448626064156923,0.));
#17348=DIRECTION('center_axis',(0.,0.,-1.));
#17349=DIRECTION('ref_axis',(-0.893719561472763,0.448626064156923,0.));
#17350=DIRECTION('',(-0.631955162396461,0.317226532182393,0.707106781186545));
#17351=DIRECTION('center_axis',(0.,0.,1.));
#17352=DIRECTION('ref_axis',(-0.893719561472762,0.448626064156926,0.));
#17353=DIRECTION('center_axis',(0.,0.,1.));
#17354=DIRECTION('ref_axis',(0.893719561472763,-0.448626064156924,0.));
#17355=DIRECTION('center_axis',(0.,0.,-1.));
#17356=DIRECTION('ref_axis',(-0.893719561472763,0.448626064156923,0.));
#17357=DIRECTION('',(0.,0.,-1.));
#17358=DIRECTION('center_axis',(0.,0.,1.));
#17359=DIRECTION('ref_axis',(0.893719561472763,-0.448626064156923,0.));
#17360=DIRECTION('',(0.,0.,-1.));
#17361=DIRECTION('center_axis',(0.,0.,-1.));
#17362=DIRECTION('ref_axis',(-0.893719561472763,0.448626064156923,0.));
#17363=DIRECTION('center_axis',(0.,0.,-1.));
#17364=DIRECTION('ref_axis',(-0.893719561472763,0.448626064156924,0.));
#17365=DIRECTION('center_axis',(0.,0.,-1.));
#17366=DIRECTION('ref_axis',(-0.893719561472763,0.448626064156924,0.));
#17367=DIRECTION('center_axis',(0.,0.,-1.));
#17368=DIRECTION('ref_axis',(-0.893719561472763,0.448626064156924,0.));
#17369=DIRECTION('axis',(0.,0.,1.));
#17370=DIRECTION('refdir',(1.,0.,0.));
#17371=DIRECTION('center_axis',(0.,0.,-1.));
#17372=DIRECTION('ref_axis',(-0.922798177671698,0.385283691954116,0.));
#17373=DIRECTION('center_axis',(0.,0.,-1.));
#17374=DIRECTION('ref_axis',(0.922798177671697,-0.385283691954117,0.));
#17375=DIRECTION('',(-0.652516849098242,0.272436711261342,0.707106781186552));
#17376=DIRECTION('center_axis',(0.,0.,1.));
#17377=DIRECTION('ref_axis',(0.922798177671698,-0.385283691954116,0.));
#17378=DIRECTION('center_axis',(0.,0.,1.));
#17379=DIRECTION('ref_axis',(0.922798177671697,-0.385283691954117,0.));
#17380=DIRECTION('center_axis',(0.,0.,1.));
#17381=DIRECTION('ref_axis',(0.922798177671697,-0.385283691954117,0.));
#17382=DIRECTION('center_axis',(0.,0.,1.));
#17383=DIRECTION('ref_axis',(0.922798177671697,-0.385283691954117,0.));
#17384=DIRECTION('',(0.652516849098248,-0.272436711261346,-0.707106781186545));
#17385=DIRECTION('center_axis',(0.,0.,-1.));
#17386=DIRECTION('ref_axis',(0.9227981776717,-0.385283691954111,0.));
#17387=DIRECTION('center_axis',(0.,0.,-1.));
#17388=DIRECTION('ref_axis',(-0.922798177671697,0.385283691954117,0.));
#17389=DIRECTION('',(0.,0.,1.));
#17390=DIRECTION('center_axis',(0.,0.,1.));
#17391=DIRECTION('ref_axis',(0.922798177671697,-0.385283691954116,0.));
#17392=DIRECTION('center_axis',(0.,0.,1.));
#17393=DIRECTION('ref_axis',(0.922798177671697,-0.385283691954116,0.));
#17394=DIRECTION('',(0.,0.,1.));
#17395=DIRECTION('',(1.,0.,0.));
#17396=DIRECTION('',(0.,0.,1.));
#17397=DIRECTION('',(1.,0.,0.));
#17398=DIRECTION('',(0.,0.,1.));
#17399=DIRECTION('',(1.,0.,0.));
#17400=DIRECTION('',(0.,0.,1.));
#17401=DIRECTION('',(1.,0.,0.));
#17402=DIRECTION('',(0.,0.,1.));
#17403=DIRECTION('',(1.,0.,0.));
#17404=DIRECTION('',(0.,0.,1.));
#17405=DIRECTION('',(1.,0.,0.));
#17406=DIRECTION('',(0.,0.,1.));
#17407=DIRECTION('',(1.,0.,0.));
#17408=DIRECTION('',(0.,0.,1.));
#17409=DIRECTION('',(1.,0.,0.));
#17410=DIRECTION('',(0.,0.,1.));
#17411=DIRECTION('',(1.,0.,0.));
#17412=DIRECTION('',(0.135281470722696,0.,0.990807208128355));
#17413=DIRECTION('',(0.990807208128355,0.,-0.135281470722696));
#17414=DIRECTION('',(0.,0.,1.));
#17415=DIRECTION('',(1.,0.,0.));
#17416=DIRECTION('',(0.,-1.22464679914735E-16,-1.));
#17417=DIRECTION('',(1.,0.,0.));
#17418=DIRECTION('',(0.,0.,1.));
#17419=DIRECTION('',(1.,0.,0.));
#17420=CARTESIAN_POINT('',(0.,0.,0.));
#17421=CARTESIAN_POINT('',(0.,0.,0.));
#17422=CARTESIAN_POINT('Origin',(37.0412526478464,187.739737607039,231.973593133701));
#17423=CARTESIAN_POINT('',(50.0412526478464,187.739737607039,231.973593133701));
#17424=CARTESIAN_POINT('Origin',(37.0412526478464,187.739737607039,231.973593133701));
#17425=CARTESIAN_POINT('',(49.4412526478464,187.739737607039,232.573593133701));
#17426=CARTESIAN_POINT('',(50.0412526478464,187.739737607039,231.973593133701));
#17427=CARTESIAN_POINT('Origin',(37.0412526478464,187.739737607039,232.573593133701));
#17428=CARTESIAN_POINT('Origin',(37.0412526478464,187.739737607039,273.573593133701));
#17429=CARTESIAN_POINT('',(24.0412526478464,187.739737607039,274.173593133701));
#17430=CARTESIAN_POINT('Origin',(37.0412526478464,187.739737607039,274.173593133701));
#17431=CARTESIAN_POINT('',(24.6412526478463,187.739737607039,273.573593133701));
#17432=CARTESIAN_POINT('',(24.6412526478463,187.739737607039,273.573593133701));
#17433=CARTESIAN_POINT('Origin',(37.0412526478464,187.739737607039,273.573593133701));
#17434=CARTESIAN_POINT('Origin',(11.0412526478464,112.739737607039,219.973593133701));
#17435=CARTESIAN_POINT('',(24.0412526478465,112.739737607039,219.973593133701));
#17436=CARTESIAN_POINT('Origin',(11.0412526478464,112.739737607039,219.973593133701));
#17437=CARTESIAN_POINT('',(23.4412526478464,112.739737607039,220.573593133701));
#17438=CARTESIAN_POINT('',(24.0412526478465,112.739737607039,219.973593133701));
#17439=CARTESIAN_POINT('Origin',(11.0412526478464,112.739737607039,220.573593133701));
#17440=CARTESIAN_POINT('Origin',(277.041252647846,78.7397376070391,221.973593133701));
#17441=CARTESIAN_POINT('',(293.041252647846,78.7397376070391,221.973593133701));
#17442=CARTESIAN_POINT('Origin',(277.041252647846,78.7397376070391,221.973593133701));
#17443=CARTESIAN_POINT('',(292.441252647846,78.7397376070391,222.573593133701));
#17444=CARTESIAN_POINT('',(293.041252647846,78.7397376070391,221.973593133701));
#17445=CARTESIAN_POINT('Origin',(277.041252647846,78.7397376070391,222.573593133701));
#17446=CARTESIAN_POINT('Origin',(11.0412526478464,112.739737607039,285.573593133701));
#17447=CARTESIAN_POINT('',(-1.95874735215359,112.739737607039,286.173593133701));
#17448=CARTESIAN_POINT('Origin',(11.0412526478464,112.739737607039,286.173593133701));
#17449=CARTESIAN_POINT('',(-1.35874735215363,112.739737607039,285.573593133701));
#17450=CARTESIAN_POINT('',(-1.35874735215363,112.739737607039,285.573593133701));
#17451=CARTESIAN_POINT('Origin',(11.0412526478464,112.739737607039,285.573593133701));
#17452=CARTESIAN_POINT('Origin',(277.041252647846,78.7397376070391,283.573593133701));
#17453=CARTESIAN_POINT('',(261.041252647846,78.7397376070391,284.173593133701));
#17454=CARTESIAN_POINT('Origin',(277.041252647846,78.7397376070391,284.173593133701));
#17455=CARTESIAN_POINT('',(261.641252647846,78.7397376070391,283.573593133701));
#17456=CARTESIAN_POINT('',(261.641252647846,78.7397376070391,283.573593133701));
#17457=CARTESIAN_POINT('Origin',(277.041252647846,78.7397376070391,283.573593133701));
#17458=CARTESIAN_POINT('Origin',(-260.909689484712,113.464793580191,211.073593133701));
#17459=CARTESIAN_POINT('',(-259.490535542311,109.194430353513,211.073593133701));
#17460=CARTESIAN_POINT('',(-256.639326258033,114.883947522592,211.073593133701));
#17461=CARTESIAN_POINT('Origin',(-260.909689484712,113.464793580191,211.073593133701));
#17462=CARTESIAN_POINT('',(-259.490535542311,109.194430353513,215.573593133701));
#17463=CARTESIAN_POINT('',(-259.490535542311,109.194430353513,211.073593133701));
#17464=CARTESIAN_POINT('',(-257.691868353316,110.319062001314,215.573593133701));
#17465=CARTESIAN_POINT('Origin',(-260.909689484712,113.464793580191,215.573593133701));
#17466=CARTESIAN_POINT('',(-256.639326258033,114.883947522592,211.573593133701));
#17467=CARTESIAN_POINT('Ctrl Pts',(-257.691868353317,110.319062001314,215.573593133701));
#17468=CARTESIAN_POINT('Ctrl Pts',(-257.226722972947,110.794866944168,215.573593133701));
#17469=CARTESIAN_POINT('Ctrl Pts',(-256.875952954917,111.37569206742,215.537123333329));
#17470=CARTESIAN_POINT('Ctrl Pts',(-256.575993830868,112.221556348799,215.307227076609));
#17471=CARTESIAN_POINT('Ctrl Pts',(-256.503984375586,112.507585568265,215.204277782028));
#17472=CARTESIAN_POINT('Ctrl Pts',(-256.419927726647,113.054277491751,214.929717220809));
#17473=CARTESIAN_POINT('Ctrl Pts',(-256.406892655266,113.314450931809,214.75743570919));
#17474=CARTESIAN_POINT('Ctrl Pts',(-256.416576787744,113.953138581935,214.220216585689));
#17475=CARTESIAN_POINT('Ctrl Pts',(-256.482778257329,114.307185871813,213.752911915794));
#17476=CARTESIAN_POINT('Ctrl Pts',(-256.596967428487,114.771542993549,212.703946142401));
#17477=CARTESIAN_POINT('Ctrl Pts',(-256.639326258033,114.883947522592,212.122608190933));
#17478=CARTESIAN_POINT('Ctrl Pts',(-256.639326258033,114.883947522592,211.573593133701));
#17479=CARTESIAN_POINT('',(-256.639326258033,114.883947522592,253.073593133701));
#17480=CARTESIAN_POINT('Origin',(203.041252647846,82.7397376070391,167.073593133701));
#17481=CARTESIAN_POINT('',(226.839232189725,88.7397376070391,163.966155326709));
#17482=CARTESIAN_POINT('',(179.041252647846,88.7397376070391,167.073593133701));
#17483=CARTESIAN_POINT('Origin',(203.041252647846,88.7397376070391,167.073593133701));
#17484=CARTESIAN_POINT('',(232.788727075195,82.7397376070391,163.189295874961));
#17485=CARTESIAN_POINT('Origin',(226.839232189725,82.7397376070391,163.966155326709));
#17486=CARTESIAN_POINT('',(173.041252647846,82.7397376070391,167.073593133701));
#17487=CARTESIAN_POINT('Origin',(203.041252647846,82.7397376070391,167.073593133701));
#17488=CARTESIAN_POINT('Origin',(179.041252647846,82.7397376070391,167.073593133701));
#17489=CARTESIAN_POINT('Origin',(277.041252647846,78.7397376070391,288.573593133701));
#17490=CARTESIAN_POINT('',(259.041252647846,78.7397376070391,290.573593133701));
#17491=CARTESIAN_POINT('Origin',(277.041252647846,78.7397376070391,290.573593133701));
#17492=CARTESIAN_POINT('',(261.041252647846,78.7397376070391,288.573593133701));
#17493=CARTESIAN_POINT('Origin',(259.041252647846,78.7397376070391,288.573593133701));
#17494=CARTESIAN_POINT('Origin',(277.041252647846,78.7397376070391,288.573593133701));
#17495=CARTESIAN_POINT('Origin',(11.0412526478464,112.739737607039,288.573593133701));
#17496=CARTESIAN_POINT('',(-3.95874735215359,112.739737607039,290.573593133701));
#17497=CARTESIAN_POINT('Origin',(11.0412526478464,112.739737607039,290.573593133701));
#17498=CARTESIAN_POINT('',(-1.95874735215359,112.739737607039,288.573593133701));
#17499=CARTESIAN_POINT('Origin',(-3.95874735215359,112.739737607039,288.573593133701));
#17500=CARTESIAN_POINT('Origin',(11.0412526478464,112.739737607039,288.573593133701));
#17501=CARTESIAN_POINT('Origin',(11.0412526478464,112.739737607039,217.573593133701));
#17502=CARTESIAN_POINT('',(26.0412526478465,112.739737607039,215.573593133701));
#17503=CARTESIAN_POINT('Origin',(11.0412526478464,112.739737607039,215.573593133701));
#17504=CARTESIAN_POINT('',(24.0412526478465,112.739737607039,217.573593133701));
#17505=CARTESIAN_POINT('Origin',(26.0412526478465,112.739737607039,217.573593133701));
#17506=CARTESIAN_POINT('Origin',(11.0412526478464,112.739737607039,217.573593133701));
#17507=CARTESIAN_POINT('Origin',(277.041252647846,78.7397376070391,217.573593133701));
#17508=CARTESIAN_POINT('',(295.041252647846,78.7397376070391,215.573593133701));
#17509=CARTESIAN_POINT('Origin',(277.041252647846,78.7397376070391,215.573593133701));
#17510=CARTESIAN_POINT('',(293.041252647846,78.7397376070391,217.573593133701));
#17511=CARTESIAN_POINT('Origin',(295.041252647846,78.7397376070391,217.573593133701));
#17512=CARTESIAN_POINT('Origin',(277.041252647846,78.7397376070391,217.573593133701));
#17513=CARTESIAN_POINT('Origin',(37.0412526478464,187.739737607039,217.573593133701));
#17514=CARTESIAN_POINT('',(41.2239632420135,202.144769092095,215.573593133701));
#17515=CARTESIAN_POINT('',(32.9752147767065,202.178135580168,215.573593133701));
#17516=CARTESIAN_POINT('Origin',(37.0412526478464,187.739737607039,215.573593133701));
#17517=CARTESIAN_POINT('',(40.6662684961245,200.224098227421,217.573593133701));
#17518=CARTESIAN_POINT('Origin',(41.2239632420135,202.144769092095,217.573593133701));
#17519=CARTESIAN_POINT('',(50.0412526478464,187.739737607039,217.573593133701));
#17520=CARTESIAN_POINT('Origin',(37.0412526478464,187.739737607039,217.573593133701));
#17521=CARTESIAN_POINT('',(33.5173531595251,200.253015850418,217.573593133701));
#17522=CARTESIAN_POINT('Origin',(37.0412526478464,187.739737607039,217.573593133701));
#17523=CARTESIAN_POINT('Origin',(32.9752147767065,202.178135580168,217.573593133701));
#17524=CARTESIAN_POINT('Origin',(37.0412526478464,187.739737607039,288.573593133701));
#17525=CARTESIAN_POINT('',(32.9752147767065,202.178135580168,290.573593133701));
#17526=CARTESIAN_POINT('',(41.2239632420135,202.144769092095,290.573593133701));
#17527=CARTESIAN_POINT('Origin',(37.0412526478464,187.739737607039,290.573593133701));
#17528=CARTESIAN_POINT('',(33.5173531595251,200.253015850418,288.573593133701));
#17529=CARTESIAN_POINT('Origin',(32.9752147767065,202.178135580168,288.573593133701));
#17530=CARTESIAN_POINT('',(24.0412526478464,187.739737607039,288.573593133701));
#17531=CARTESIAN_POINT('Origin',(37.0412526478464,187.739737607039,288.573593133701));
#17532=CARTESIAN_POINT('',(40.6662684961245,200.224098227421,288.573593133701));
#17533=CARTESIAN_POINT('Origin',(37.0412526478464,187.739737607039,288.573593133701));
#17534=CARTESIAN_POINT('Origin',(41.2239632420135,202.144769092095,288.573593133701));
#17535=CARTESIAN_POINT('Origin',(-276.958747352154,52.7397376070391,288.573593133701));
#17536=CARTESIAN_POINT('',(-288.458747352154,52.7397376070391,290.573593133701));
#17537=CARTESIAN_POINT('Origin',(-276.958747352154,52.7397376070391,290.573593133701));
#17538=CARTESIAN_POINT('',(-286.458747352154,52.7397376070391,288.573593133701));
#17539=CARTESIAN_POINT('Origin',(-288.458747352154,52.7397376070391,288.573593133701));
#17540=CARTESIAN_POINT('',(-267.458747352154,52.7397376070391,288.573593133701));
#17541=CARTESIAN_POINT('Origin',(-276.958747352154,52.7397376070391,288.573593133701));
#17542=CARTESIAN_POINT('Origin',(-276.958747352154,52.7397376070391,288.573593133701));
#17543=CARTESIAN_POINT('Origin',(-276.958747352154,52.7397376070391,217.573593133701));
#17544=CARTESIAN_POINT('',(-265.458747352154,52.7397376070391,215.573593133701));
#17545=CARTESIAN_POINT('Origin',(-276.958747352154,52.7397376070391,215.573593133701));
#17546=CARTESIAN_POINT('',(-267.458747352154,52.7397376070391,217.573593133701));
#17547=CARTESIAN_POINT('Origin',(-265.458747352154,52.7397376070391,217.573593133701));
#17548=CARTESIAN_POINT('Origin',(-276.958747352154,52.7397376070391,217.573593133701));
#17549=CARTESIAN_POINT('Origin',(-276.958747352154,52.7397376070391,297.073593133701));
#17550=CARTESIAN_POINT('',(-267.458747352154,52.7397376070391,297.073593133701));
#17551=CARTESIAN_POINT('',(-286.458747352154,52.7397376070391,297.073593133701));
#17552=CARTESIAN_POINT('Origin',(-276.958747352154,52.7397376070391,297.073593133701));
#17553=CARTESIAN_POINT('Origin',(-276.958747352154,52.7397376070391,297.073593133701));
#17554=CARTESIAN_POINT('',(-288.458747352154,52.7397376070391,295.073593133701));
#17555=CARTESIAN_POINT('Origin',(-288.458747352154,52.7397376070391,297.073593133701));
#17556=CARTESIAN_POINT('Origin',(-276.958747352154,52.7397376070391,295.073593133701));
#17557=CARTESIAN_POINT('Origin',(-276.958747352154,52.7397376070391,209.073593133701));
#17558=CARTESIAN_POINT('',(-286.458747352154,52.7397376070391,209.073593133701));
#17559=CARTESIAN_POINT('',(-267.458747352154,52.7397376070391,209.073593133701));
#17560=CARTESIAN_POINT('Origin',(-276.958747352154,52.7397376070391,209.073593133701));
#17561=CARTESIAN_POINT('Origin',(-276.958747352154,52.7397376070391,209.073593133701));
#17562=CARTESIAN_POINT('',(-265.458747352154,52.7397376070391,211.073593133701));
#17563=CARTESIAN_POINT('Origin',(-265.458747352154,52.7397376070391,209.073593133701));
#17564=CARTESIAN_POINT('Origin',(-276.958747352154,52.7397376070391,211.073593133701));
#17565=CARTESIAN_POINT('Origin',(231.506382410955,182.009983898606,207.432430075574));
#17566=CARTESIAN_POINT('',(231.480498531968,37.7397376070391,211.432346327798));
#17567=CARTESIAN_POINT('',(233.162260300213,37.7397376070391,211.073593133701));
#17568=CARTESIAN_POINT('Origin',(231.506382410955,37.7397376070391,207.432430075574));
#17569=CARTESIAN_POINT('',(231.480498531968,85.7397376070391,211.432346327798));
#17570=CARTESIAN_POINT('',(231.480498531968,37.7397376070391,211.432346327798));
#17571=CARTESIAN_POINT('',(232.024288712121,85.7397376070391,211.39875999922));
#17572=CARTESIAN_POINT('Origin',(231.506382410955,85.7397376070391,207.432430075574));
#17573=CARTESIAN_POINT('',(235.472712334602,81.7397376070391,206.914523774409));
#17574=CARTESIAN_POINT('Origin',(231.506382410961,81.739737607044,207.432430075578));
#17575=CARTESIAN_POINT('',(235.472712334602,37.7397376070391,206.914523774409));
#17576=CARTESIAN_POINT('',(235.472712334602,85.7397376070391,206.914523774409));
#17577=CARTESIAN_POINT('Origin',(231.506382410955,37.7397376070391,207.432430075574));
#17578=CARTESIAN_POINT('Origin',(203.041252647846,81.7397376070391,167.073593133701));
#17579=CARTESIAN_POINT('',(180.041252647846,85.7397376070391,167.073593133701));
#17580=CARTESIAN_POINT('',(225.847649708814,85.7397376070391,164.095631902));
#17581=CARTESIAN_POINT('Origin',(203.041252647846,85.7397376070391,167.073593133701));
#17582=CARTESIAN_POINT('',(176.041252647846,81.7397376070391,167.073593133701));
#17583=CARTESIAN_POINT('Origin',(180.041252647846,81.7397376070391,167.073593133701));
#17584=CARTESIAN_POINT('',(229.81397963246,81.7397376070391,163.577725600835));
#17585=CARTESIAN_POINT('Origin',(203.041252647846,81.7397376070391,167.073593133701));
#17586=CARTESIAN_POINT('Origin',(225.847649708814,81.7397376070391,164.095631902));
#17587=CARTESIAN_POINT('Origin',(-276.958747352154,52.7397376070391,137.073593133701));
#17588=CARTESIAN_POINT('',(-282.958747352154,52.7397376070391,198.823593133701));
#17589=CARTESIAN_POINT('Origin',(-276.958747352154,52.7397376070391,198.823593133701));
#17590=CARTESIAN_POINT('',(-282.958747352154,52.7397376070391,307.323593133701));
#17591=CARTESIAN_POINT('',(-282.958747352154,52.7397376070391,137.073593133701));
#17592=CARTESIAN_POINT('Origin',(-276.958747352154,52.7397376070391,307.323593133701));
#17593=CARTESIAN_POINT('Origin',(11.0412526478464,112.739737607039,220.573593133701));
#17594=CARTESIAN_POINT('',(24.0412526478465,112.739737607039,220.573593133701));
#17595=CARTESIAN_POINT('Origin',(37.0412526478464,187.739737607039,232.573593133701));
#17596=CARTESIAN_POINT('',(50.0412526478464,187.739737607039,232.573593133701));
#17597=CARTESIAN_POINT('Ctrl Pts',(40.6662684961245,200.224098227421,217.573593133701));
#17598=CARTESIAN_POINT('Ctrl Pts',(40.0831826062374,200.393405703872,217.573593133701));
#17599=CARTESIAN_POINT('Ctrl Pts',(39.4921714450088,200.520958444757,217.554555800012));
#17600=CARTESIAN_POINT('Ctrl Pts',(38.5932073487587,200.650318107912,217.531285607299));
#17601=CARTESIAN_POINT('Ctrl Pts',(38.290917247095,200.68305475883,217.524189505008));
#17602=CARTESIAN_POINT('Ctrl Pts',(37.688803228723,200.727108347403,217.514471384328));
#17603=CARTESIAN_POINT('Ctrl Pts',(37.3882478564454,200.73856950399,217.511826783315));
#17604=CARTESIAN_POINT('Ctrl Pts',(36.4880719422569,200.741819615196,217.511924454037));
#17605=CARTESIAN_POINT('Ctrl Pts',(35.8899421476187,200.7026257403,217.523628183181));
#17606=CARTESIAN_POINT('Ctrl Pts',(34.6975601484818,200.540873888315,217.55445906248));
#17607=CARTESIAN_POINT('Ctrl Pts',(34.101487070175,200.417515444274,217.573593133701));
#17608=CARTESIAN_POINT('Ctrl Pts',(33.5173531595251,200.253015850418,217.573593133701));
#17609=CARTESIAN_POINT('Origin',(277.041252647846,78.7397376070391,222.573593133701));
#17610=CARTESIAN_POINT('',(293.041252647846,78.7397376070391,222.573593133701));
#17611=CARTESIAN_POINT('Origin',(203.041252647846,182.009983898606,167.073593133701));
#17612=CARTESIAN_POINT('',(176.041252647846,70.8334876070391,167.073593133701));
#17613=CARTESIAN_POINT('',(176.041252647846,182.009983898606,167.073593133701));
#17614=CARTESIAN_POINT('',(229.81397963246,71.8713232808586,163.577725600835));
#17615=CARTESIAN_POINT('Origin',(203.041252647847,70.8334876070393,167.0735931337));
#17616=CARTESIAN_POINT('',(229.81397963246,182.009983898606,163.577725600835));
#17617=CARTESIAN_POINT('Origin',(-276.958747352154,52.7397376070391,198.823593133701));
#17618=CARTESIAN_POINT('',(-286.458747352154,52.7397376070391,198.823593133701));
#17619=CARTESIAN_POINT('',(-286.458747352154,52.7397376070391,198.823593133701));
#17620=CARTESIAN_POINT('Origin',(-276.958747352154,52.7397376070391,198.823593133701));
#17621=CARTESIAN_POINT('Origin',(11.0412526478464,112.739737607039,211.073593133701));
#17622=CARTESIAN_POINT('',(5.04125264784645,112.739737607039,211.073593133701));
#17623=CARTESIAN_POINT('Origin',(11.0412526478464,112.739737607039,211.073593133701));
#17624=CARTESIAN_POINT('',(5.04125264784645,112.739737607039,220.573593133701));
#17625=CARTESIAN_POINT('',(5.04125264784645,112.739737607039,211.073593133701));
#17626=CARTESIAN_POINT('Origin',(11.0412526478464,112.739737607039,220.573593133701));
#17627=CARTESIAN_POINT('Origin',(277.041252647846,78.7397376070391,211.073593133701));
#17628=CARTESIAN_POINT('',(269.041252647846,78.7397376070391,211.073593133701));
#17629=CARTESIAN_POINT('Origin',(277.041252647846,78.7397376070391,211.073593133701));
#17630=CARTESIAN_POINT('',(269.041252647846,78.7397376070391,222.573593133701));
#17631=CARTESIAN_POINT('',(269.041252647846,78.7397376070391,211.073593133701));
#17632=CARTESIAN_POINT('Origin',(277.041252647846,78.7397376070391,222.573593133701));
#17633=CARTESIAN_POINT('Origin',(37.0412526478464,187.739737607039,211.073593133701));
#17634=CARTESIAN_POINT('',(29.0412526478464,187.739737607039,211.073593133701));
#17635=CARTESIAN_POINT('Origin',(37.0412526478464,187.739737607039,211.073593133701));
#17636=CARTESIAN_POINT('',(29.0412526478464,187.739737607039,232.573593133701));
#17637=CARTESIAN_POINT('',(29.0412526478464,187.739737607039,211.073593133701));
#17638=CARTESIAN_POINT('Origin',(37.0412526478464,187.739737607039,232.573593133701));
#17639=CARTESIAN_POINT('Origin',(11.0412526478464,112.739737607039,285.573593133701));
#17640=CARTESIAN_POINT('',(-1.95874735215359,112.739737607039,285.573593133701));
#17641=CARTESIAN_POINT('Origin',(37.0412526478464,187.739737607039,273.573593133701));
#17642=CARTESIAN_POINT('',(24.0412526478464,187.739737607039,273.573593133701));
#17643=CARTESIAN_POINT('Ctrl Pts',(33.5173531595251,200.253015850418,288.573593133701));
#17644=CARTESIAN_POINT('Ctrl Pts',(34.1017896558591,200.41760065628,288.573593133701));
#17645=CARTESIAN_POINT('Ctrl Pts',(34.6938133708609,200.540367977988,288.59263046739));
#17646=CARTESIAN_POINT('Ctrl Pts',(35.5937945612941,200.662450841916,288.615900660103));
#17647=CARTESIAN_POINT('Ctrl Pts',(35.896339608343,200.692740912621,288.622996762393));
#17648=CARTESIAN_POINT('Ctrl Pts',(36.4987903139835,200.731921992999,288.632714883073));
#17649=CARTESIAN_POINT('Ctrl Pts',(36.7994285709306,200.740951299452,288.635359484086));
#17650=CARTESIAN_POINT('Ctrl Pts',(37.6996013208751,200.736918934719,288.635261813365));
#17651=CARTESIAN_POINT('Ctrl Pts',(38.2973944661359,200.69288750796,288.62355808422));
#17652=CARTESIAN_POINT('Ctrl Pts',(39.4884288827824,200.521494649736,288.592727204922));
#17653=CARTESIAN_POINT('Ctrl Pts',(40.0834844926596,200.393318046755,288.573593133701));
#17654=CARTESIAN_POINT('Ctrl Pts',(40.6662684961245,200.224098227421,288.573593133701));
#17655=CARTESIAN_POINT('Origin',(277.041252647846,78.7397376070391,283.573593133701));
#17656=CARTESIAN_POINT('',(261.041252647846,78.7397376070391,283.573593133701));
#17657=CARTESIAN_POINT('Origin',(-276.958747352154,52.7397376070391,307.323593133701));
#17658=CARTESIAN_POINT('',(-267.458747352154,52.7397376070391,307.323593133701));
#17659=CARTESIAN_POINT('',(-267.458747352154,52.7397376070391,307.323593133701));
#17660=CARTESIAN_POINT('Origin',(-276.958747352154,52.7397376070391,307.323593133701));
#17661=CARTESIAN_POINT('Origin',(11.0412526478464,112.739737607039,295.073593133701));
#17662=CARTESIAN_POINT('',(17.0412526478464,112.739737607039,295.073593133701));
#17663=CARTESIAN_POINT('Origin',(11.0412526478464,112.739737607039,295.073593133701));
#17664=CARTESIAN_POINT('',(17.0412526478464,112.739737607039,285.573593133701));
#17665=CARTESIAN_POINT('',(17.0412526478464,112.739737607039,295.073593133701));
#17666=CARTESIAN_POINT('Origin',(11.0412526478464,112.739737607039,285.573593133701));
#17667=CARTESIAN_POINT('Origin',(277.041252647846,78.7397376070391,295.073593133701));
#17668=CARTESIAN_POINT('',(285.041252647846,78.7397376070391,295.073593133701));
#17669=CARTESIAN_POINT('Origin',(277.041252647846,78.7397376070391,295.073593133701));
#17670=CARTESIAN_POINT('',(285.041252647846,78.7397376070391,283.573593133701));
#17671=CARTESIAN_POINT('',(285.041252647846,78.7397376070391,295.073593133701));
#17672=CARTESIAN_POINT('Origin',(277.041252647846,78.7397376070391,283.573593133701));
#17673=CARTESIAN_POINT('Origin',(37.0412526478464,187.739737607039,295.073593133701));
#17674=CARTESIAN_POINT('',(45.0412526478464,187.739737607039,295.073593133701));
#17675=CARTESIAN_POINT('Origin',(37.0412526478464,187.739737607039,295.073593133701));
#17676=CARTESIAN_POINT('',(45.0412526478464,187.739737607039,273.573593133701));
#17677=CARTESIAN_POINT('',(45.0412526478464,187.739737607039,295.073593133701));
#17678=CARTESIAN_POINT('Origin',(37.0412526478464,187.739737607039,273.573593133701));
#17679=CARTESIAN_POINT('Origin',(-276.958747352154,52.7397376070391,290.573593133701));
#17680=CARTESIAN_POINT('',(-267.458747352154,52.7397376070391,290.573593133701));
#17681=CARTESIAN_POINT('Origin',(203.041252647846,88.7397376070391,339.073593133701));
#17682=CARTESIAN_POINT('',(203.041252647846,88.7397376070391,344.073593133701));
#17683=CARTESIAN_POINT('Origin',(203.041252647846,88.7397376070391,339.073593133701));
#17684=CARTESIAN_POINT('',(203.041252647846,85.7397376070391,344.073593133701));
#17685=CARTESIAN_POINT('',(203.041252647846,88.7397376070391,344.073593133701));
#17686=CARTESIAN_POINT('Origin',(203.041252647846,85.7397376070391,339.073593133701));
#17687=CARTESIAN_POINT('Origin',(203.041252647846,88.7397376070391,167.073593133701));
#17688=CARTESIAN_POINT('',(232.788727075195,71.9866383557274,163.189295874961));
#17689=CARTESIAN_POINT('',(232.788727075195,88.7397376070391,163.189295874961));
#17690=CARTESIAN_POINT('',(173.041252647846,70.8334876070391,167.073593133701));
#17691=CARTESIAN_POINT('Origin',(203.041252647851,70.8334876070379,167.073593133705));
#17692=CARTESIAN_POINT('',(173.041252647846,88.7397376070391,167.073593133701));
#17693=CARTESIAN_POINT('Origin',(203.041252647846,88.7397376070391,167.073593133701));
#17694=CARTESIAN_POINT('',(203.041252647846,88.7397376070391,172.073593133701));
#17695=CARTESIAN_POINT('Origin',(203.041252647846,88.7397376070391,167.073593133701));
#17696=CARTESIAN_POINT('',(203.041252647846,85.7397376070391,172.073593133701));
#17697=CARTESIAN_POINT('',(203.041252647846,88.7397376070391,172.073593133701));
#17698=CARTESIAN_POINT('Origin',(203.041252647846,85.7397376070391,167.073593133701));
#17699=CARTESIAN_POINT('Origin',(-293.958747352154,37.7397376070391,211.073593133701));
#17700=CARTESIAN_POINT('',(173.041252647846,37.7397376070391,203.073593133701));
#17701=CARTESIAN_POINT('',(173.041252647846,37.7397376070391,211.073593133701));
#17702=CARTESIAN_POINT('',(173.041252647846,37.7397376070391,167.073593133701));
#17703=CARTESIAN_POINT('',(176.041252647846,37.7397376070391,203.073593133701));
#17704=CARTESIAN_POINT('',(-293.958747352154,37.7397376070391,203.073593133701));
#17705=CARTESIAN_POINT('',(176.041252647846,37.7397376070391,207.0993938051));
#17706=CARTESIAN_POINT('',(176.041252647846,37.7397376070391,167.073593133701));
#17707=CARTESIAN_POINT('',(179.587667268292,37.7397376070391,211.073593133701));
#17708=CARTESIAN_POINT('Origin',(180.041252647846,37.7397376070391,207.0993938051));
#17709=CARTESIAN_POINT('',(82.0412526478464,37.7397376070391,211.073593133701));
#17710=CARTESIAN_POINT('Origin',(-293.958747352154,37.7397376070391,211.073593133701));
#17711=CARTESIAN_POINT('',(-278.958747352154,37.7397376070391,211.073593133701));
#17712=CARTESIAN_POINT('',(80.0412526478464,37.7397376070391,211.073593133701));
#17713=CARTESIAN_POINT('',(-293.958747352154,37.7397376070391,211.073593133701));
#17714=CARTESIAN_POINT('',(80.0412526478464,37.7397376070391,215.573593133701));
#17715=CARTESIAN_POINT('',(80.0412526478464,37.7397376070391,211.073593133701));
#17716=CARTESIAN_POINT('',(-278.958747352154,37.7397376070391,215.573593133701));
#17717=CARTESIAN_POINT('',(-293.958747352154,37.7397376070391,215.573593133701));
#17718=CARTESIAN_POINT('',(-278.958747352154,37.7397376070391,211.073593133701));
#17719=CARTESIAN_POINT('Origin',(-293.958747352154,37.7397376070391,211.073593133701));
#17720=CARTESIAN_POINT('',(234.971180132426,37.7397376070391,203.073593133701));
#17721=CARTESIAN_POINT('',(234.760748217833,37.7397376070391,201.462022859575));
#17722=CARTESIAN_POINT('',(237.996647058024,37.7397376070391,203.073593133701));
#17723=CARTESIAN_POINT('',(-293.958747352154,37.7397376070391,203.073593133701));
#17724=CARTESIAN_POINT('',(239.041252647847,37.7397376070391,211.073593133701));
#17725=CARTESIAN_POINT('',(239.041252647847,37.7397376070391,211.073593133701));
#17726=CARTESIAN_POINT('',(82.0412526478464,37.7397376070391,211.073593133701));
#17727=CARTESIAN_POINT('Origin',(-293.958747352154,37.7397376070391,295.073593133701));
#17728=CARTESIAN_POINT('',(176.041252647846,37.7397376070391,303.073593133701));
#17729=CARTESIAN_POINT('',(176.041252647846,37.7397376070391,299.047792462302));
#17730=CARTESIAN_POINT('',(176.041252647846,37.7397376070391,305.073593133701));
#17731=CARTESIAN_POINT('',(173.041252647846,37.7397376070391,303.073593133701));
#17732=CARTESIAN_POINT('',(-293.958747352154,37.7397376070391,303.073593133701));
#17733=CARTESIAN_POINT('',(173.041252647846,37.7397376070391,295.073593133701));
#17734=CARTESIAN_POINT('',(173.041252647846,37.7397376070391,339.073593133701));
#17735=CARTESIAN_POINT('',(179.587667268292,37.7397376070391,295.073593133701));
#17736=CARTESIAN_POINT('',(82.0412526478464,37.7397376070391,295.073593133701));
#17737=CARTESIAN_POINT('Origin',(180.041252647846,37.7397376070391,299.047792462302));
#17738=CARTESIAN_POINT('Origin',(-293.958747352154,37.7397376070391,295.073593133701));
#17739=CARTESIAN_POINT('',(-278.958747352154,37.7397376070391,290.573593133701));
#17740=CARTESIAN_POINT('',(80.0412526478464,37.7397376070391,290.573593133701));
#17741=CARTESIAN_POINT('',(-293.958747352154,37.7397376070391,290.573593133701));
#17742=CARTESIAN_POINT('',(80.0412526478464,37.7397376070391,295.073593133701));
#17743=CARTESIAN_POINT('',(80.0412526478464,37.7397376070391,295.073593133701));
#17744=CARTESIAN_POINT('',(-278.958747352154,37.7397376070391,295.073593133701));
#17745=CARTESIAN_POINT('',(-293.958747352154,37.7397376070391,295.073593133701));
#17746=CARTESIAN_POINT('',(-278.958747352154,37.7397376070391,295.073593133701));
#17747=CARTESIAN_POINT('Origin',(-293.958747352154,37.7397376070391,295.073593133701));
#17748=CARTESIAN_POINT('',(239.041252647847,37.7397376070391,295.073593133701));
#17749=CARTESIAN_POINT('',(237.996647058024,37.7397376070391,303.073593133701));
#17750=CARTESIAN_POINT('',(239.041252647847,37.7397376070391,295.073593133701));
#17751=CARTESIAN_POINT('',(234.971180132426,37.7397376070391,303.073593133701));
#17752=CARTESIAN_POINT('',(-293.958747352154,37.7397376070391,303.073593133701));
#17753=CARTESIAN_POINT('',(235.472712334602,37.7397376070391,299.232662492993));
#17754=CARTESIAN_POINT('',(233.826607434235,37.7397376070391,311.839180523564));
#17755=CARTESIAN_POINT('',(233.162260300213,37.7397376070391,295.073593133701));
#17756=CARTESIAN_POINT('Origin',(231.506382410955,37.7397376070391,298.714756191828));
#17757=CARTESIAN_POINT('',(82.0412526478464,37.7397376070391,295.073593133701));
#17758=CARTESIAN_POINT('Origin',(36.6954328642313,102.247359653123,211.073593133701));
#17759=CARTESIAN_POINT('',(19.2205075843702,200.70865654923,214.922518540102));
#17760=CARTESIAN_POINT('',(14.7441480327787,199.808320566024,210.390652633755));
#17761=CARTESIAN_POINT('Origin',(36.6954317604653,102.24736509754,200.454194907216));
#17762=CARTESIAN_POINT('',(19.2205075843702,200.70865654923,215.573593133701));
#17763=CARTESIAN_POINT('',(19.2205075843702,200.70865654923,211.073593133701));
#17764=CARTESIAN_POINT('Origin',(36.6954328642313,102.247359653123,215.573593133701));
#17765=CARTESIAN_POINT('Origin',(36.6954328642313,102.247359653123,215.573593133701));
#17766=CARTESIAN_POINT('',(68.8536755000203,196.935518525169,215.573593133701));
#17767=CARTESIAN_POINT('Origin',(36.6954328642313,102.247359653123,215.573593133701));
#17768=CARTESIAN_POINT('',(68.8536755000203,196.935518525169,211.073593133701));
#17769=CARTESIAN_POINT('',(68.8536755000203,196.935518525169,211.073593133701));
#17770=CARTESIAN_POINT('',(24.6736703960697,201.522115896385,211.073593133701));
#17771=CARTESIAN_POINT('Origin',(36.6954328642313,102.247359653123,211.073593133701));
#17772=CARTESIAN_POINT('Ctrl Pts',(24.6736703960694,201.522115896385,211.073593133701));
#17773=CARTESIAN_POINT('Ctrl Pts',(21.5391004439812,201.142532437006,211.073593133701));
#17774=CARTESIAN_POINT('Ctrl Pts',(18.1382702274613,200.570522874585,210.784723883084));
#17775=CARTESIAN_POINT('Ctrl Pts',(14.7712835464547,199.814423097892,210.39380950634));
#17776=CARTESIAN_POINT('Ctrl Pts',(14.7577154236595,199.811373238515,210.392231751654));
#17777=CARTESIAN_POINT('Ctrl Pts',(14.7441480327787,199.808320566023,210.390652633755));
#17778=CARTESIAN_POINT('Origin',(-292.116850606278,98.3518483080855,253.073593133701));
#17779=CARTESIAN_POINT('',(10.5134668616108,198.923857134272,206.096933730814));
#17780=CARTESIAN_POINT('',(13.3382261621522,199.862598895781,209.073593133701));
#17781=CARTESIAN_POINT('',(-118.511980891635,156.045309542559,70.1332032307269));
#17782=CARTESIAN_POINT('',(-253.322233103775,111.244319381425,209.073593133701));
#17783=CARTESIAN_POINT('',(-292.116850606278,98.3518483080855,209.073593133701));
#17784=CARTESIAN_POINT('',(-250.497473803234,112.183061142934,206.096933730814));
#17785=CARTESIAN_POINT('',(-293.596873185455,97.8599979041293,251.513983036674));
#17786=CARTESIAN_POINT('',(-214.933263098157,124.001983129515,190.573593133701));
#17787=CARTESIAN_POINT('Origin',(-214.933263098157,124.001983129515,243.573593133701));
#17788=CARTESIAN_POINT('',(-25.0507438434661,187.104935147691,190.573593133701));
#17789=CARTESIAN_POINT('',(-292.116850606278,98.3518483080855,190.573593133701));
#17790=CARTESIAN_POINT('Origin',(-25.0507438434661,187.104935147691,243.573593133701));
#17791=CARTESIAN_POINT('Origin',(-293.958747352154,37.7397376070391,211.073593133701));
#17792=CARTESIAN_POINT('',(264.041252647846,37.7397376070391,215.573593133701));
#17793=CARTESIAN_POINT('',(287.041252647846,37.7397376070391,215.573593133701));
#17794=CARTESIAN_POINT('',(-293.958747352154,37.7397376070391,215.573593133701));
#17795=CARTESIAN_POINT('',(264.041252647846,37.7397376070391,211.073593133701));
#17796=CARTESIAN_POINT('',(264.041252647846,37.7397376070391,211.073593133701));
#17797=CARTESIAN_POINT('',(287.041252647846,37.7397376070391,211.073593133701));
#17798=CARTESIAN_POINT('',(-293.958747352154,37.7397376070391,211.073593133701));
#17799=CARTESIAN_POINT('',(287.041252647846,37.7397376070391,211.073593133701));
#17800=CARTESIAN_POINT('Origin',(-293.959747352154,79.7397376070391,137.073593133701));
#17801=CARTESIAN_POINT('',(176.041252647846,62.8635864382735,193.919576017964));
#17802=CARTESIAN_POINT('',(176.041252647846,79.7397376070391,137.073593133701));
#17803=CARTESIAN_POINT('',(173.041252647846,62.8635864382735,193.919576017964));
#17804=CARTESIAN_POINT('',(-293.959747352154,62.8635864382735,193.919576017964));
#17805=CARTESIAN_POINT('',(173.041252647846,79.7397376070394,137.0735931337));
#17806=CARTESIAN_POINT('',(236.80135487697,62.8635864382735,193.919576017964));
#17807=CARTESIAN_POINT('',(221.30495438235,98.0959760916413,75.2420529750407));
#17808=CARTESIAN_POINT('',(233.775887951372,62.8635864382735,193.919576017964));
#17809=CARTESIAN_POINT('',(-293.959747352154,62.8635864382735,193.919576017964));
#17810=CARTESIAN_POINT('',(218.326162231598,97.9898570057988,75.5995067378785));
#17811=CARTESIAN_POINT('Origin',(-293.959747352154,53.2771177754925,191.073593133701));
#17812=CARTESIAN_POINT('',(176.041252647846,53.2771177754925,201.073593133701));
#17813=CARTESIAN_POINT('Origin',(176.041252647846,53.2771177754925,191.073593133701));
#17814=CARTESIAN_POINT('',(173.041252647846,53.2771177754925,201.073593133701));
#17815=CARTESIAN_POINT('',(-293.959747352154,53.2771177754925,201.073593133701));
#17816=CARTESIAN_POINT('Origin',(173.041252647846,53.2771177754925,191.073593133701));
#17817=CARTESIAN_POINT('Origin',(-293.959747352154,53.2771177754925,191.073593133701));
#17818=CARTESIAN_POINT('',(234.71002873497,53.2771177754925,201.073593133701));
#17819=CARTESIAN_POINT('',(237.735495660568,53.2771177754925,201.073593133701));
#17820=CARTESIAN_POINT('',(-293.959747352154,53.2771177754925,201.073593133701));
#17821=CARTESIAN_POINT('Origin',(233.404271747693,53.277117775496,191.073593133705));
#17822=CARTESIAN_POINT('Origin',(236.42973867329,53.2771177754941,191.073593133703));
#17823=CARTESIAN_POINT('Origin',(-293.959747352154,53.2771177754925,201.073593133701));
#17824=CARTESIAN_POINT('',(176.041252647846,39.7397376070391,201.073593133701));
#17825=CARTESIAN_POINT('',(176.041252647846,53.2771177754925,201.073593133701));
#17826=CARTESIAN_POINT('',(173.041252647846,39.7397376070391,201.073593133701));
#17827=CARTESIAN_POINT('',(-293.959747352154,39.7397376070391,201.073593133701));
#17828=CARTESIAN_POINT('',(173.041252647846,53.2771177754925,201.073593133701));
#17829=CARTESIAN_POINT('Origin',(-293.959747352154,53.2771177754925,201.073593133701));
#17830=CARTESIAN_POINT('',(237.735495660568,39.7397376070391,201.073593133701));
#17831=CARTESIAN_POINT('',(237.735495660568,53.2771177754925,201.073593133701));
#17832=CARTESIAN_POINT('',(234.71002873497,39.7397376070391,201.073593133701));
#17833=CARTESIAN_POINT('',(-293.959747352154,39.7397376070391,201.073593133701));
#17834=CARTESIAN_POINT('',(234.71002873497,53.2771177754925,201.073593133701));
#17835=CARTESIAN_POINT('Origin',(173.041252647846,88.7397376070391,167.073593133701));
#17836=CARTESIAN_POINT('',(173.041252647846,82.7397376070391,211.073593133701));
#17837=CARTESIAN_POINT('',(173.041252647846,88.7397376070391,211.073593133701));
#17838=CARTESIAN_POINT('',(173.041252647846,82.7397376070391,167.073593133701));
#17839=CARTESIAN_POINT('Origin',(173.041252647846,39.7397376070391,203.073593133701));
#17840=CARTESIAN_POINT('Origin',(239.041252647847,88.7397376070391,211.073593133701));
#17841=CARTESIAN_POINT('',(239.041252647847,82.7397376070391,211.073593133701));
#17842=CARTESIAN_POINT('',(239.041252647847,82.7397376070391,211.073593133701));
#17843=CARTESIAN_POINT('',(239.041252647847,88.7397376070391,211.073593133701));
#17844=CARTESIAN_POINT('Origin',(237.996647058024,39.7397376070393,203.073593133701));
#17845=CARTESIAN_POINT('Origin',(-276.958747352154,52.7397376070391,211.073593133701));
#17846=CARTESIAN_POINT('',(262.309201840278,36.7397376070391,211.073593133701));
#17847=CARTESIAN_POINT('Origin',(264.041252647846,35.7397376070391,211.073593133701));
#17848=CARTESIAN_POINT('',(81.7733034554153,36.7397376070391,211.073593133701));
#17849=CARTESIAN_POINT('',(-276.958747352154,36.7397376070391,211.073593133701));
#17850=CARTESIAN_POINT('Origin',(80.0412526478464,35.7397376070391,211.073593133701));
#17851=CARTESIAN_POINT('',(-293.958747352154,52.7397376070391,211.073593133701));
#17852=CARTESIAN_POINT('Origin',(-278.958747352154,52.7397376070391,211.073593133701));
#17853=CARTESIAN_POINT('',(-293.958747352154,86.9180139243132,211.073593133701));
#17854=CARTESIAN_POINT('',(-293.958747352154,97.7397376070391,211.073593133701));
#17855=CARTESIAN_POINT('',(-283.689260493489,101.152558013242,211.073593133701));
#17856=CARTESIAN_POINT('Origin',(-278.958747352154,86.9180139243132,211.073593133701));
#17857=CARTESIAN_POINT('',(37.0412526478464,207.739737607039,211.073593133701));
#17858=CARTESIAN_POINT('',(-254.589437230121,108.715645084056,211.073593133701));
#17859=CARTESIAN_POINT('',(-256.639326258033,114.883947522592,211.073593133701));
#17860=CARTESIAN_POINT('',(-291.486115520766,96.4539090962283,211.073593133701));
#17861=CARTESIAN_POINT('',(291.864989043215,121.19582713314,211.073593133701));
#17862=CARTESIAN_POINT('',(302.041252647846,117.739737607039,211.073593133701));
#17863=CARTESIAN_POINT('',(302.041252647846,106.992603302334,211.073593133701));
#17864=CARTESIAN_POINT('Origin',(287.041252647846,106.992603302334,211.073593133701));
#17865=CARTESIAN_POINT('',(302.041252647846,52.7397376070391,211.073593133701));
#17866=CARTESIAN_POINT('',(302.041252647846,37.7397376070391,211.073593133701));
#17867=CARTESIAN_POINT('Origin',(287.041252647846,52.7397376070391,211.073593133701));
#17868=CARTESIAN_POINT('',(179.041252647847,88.7397376070391,211.073593133701));
#17869=CARTESIAN_POINT('',(232.990318796651,88.7397376070391,211.073593133701));
#17870=CARTESIAN_POINT('',(173.041252647846,88.7397376070391,211.073593133701));
#17871=CARTESIAN_POINT('Origin',(179.041252647847,82.7397376070391,211.073593133701));
#17872=CARTESIAN_POINT('',(82.0412526478464,37.7397376070391,211.073593133701));
#17873=CARTESIAN_POINT('Origin',(232.990318796656,82.7397376070436,211.073593133701));
#17874=CARTESIAN_POINT('Origin',(-276.958747352154,52.7397376070391,290.573593133701));
#17875=CARTESIAN_POINT('',(264.041252647846,37.7397376070391,290.573593133701));
#17876=CARTESIAN_POINT('',(287.041252647846,37.7397376070391,290.573593133701));
#17877=CARTESIAN_POINT('',(-293.958747352154,37.7397376070391,290.573593133701));
#17878=CARTESIAN_POINT('',(262.309201840278,36.7397376070391,290.573593133701));
#17879=CARTESIAN_POINT('Origin',(264.041252647846,35.7397376070391,290.573593133701));
#17880=CARTESIAN_POINT('',(81.7733034554153,36.7397376070391,290.573593133701));
#17881=CARTESIAN_POINT('',(-276.958747352154,36.7397376070391,290.573593133701));
#17882=CARTESIAN_POINT('Origin',(80.0412526478464,35.7397376070391,290.573593133701));
#17883=CARTESIAN_POINT('',(-293.958747352154,52.7397376070391,290.573593133701));
#17884=CARTESIAN_POINT('Origin',(-278.958747352154,52.7397376070391,290.573593133701));
#17885=CARTESIAN_POINT('',(-293.958747352154,86.9180139243132,290.573593133701));
#17886=CARTESIAN_POINT('',(-293.958747352154,97.7397376070391,290.573593133701));
#17887=CARTESIAN_POINT('',(-283.689260493489,101.152558013242,290.573593133701));
#17888=CARTESIAN_POINT('Origin',(-278.958747352154,86.9180139243132,290.573593133701));
#17889=CARTESIAN_POINT('',(-259.490535542311,109.194430353513,290.573593133701));
#17890=CARTESIAN_POINT('',(37.0412526478464,207.739737607039,290.573593133701));
#17891=CARTESIAN_POINT('',(-257.691868353317,110.319062001314,290.573593133701));
#17892=CARTESIAN_POINT('Origin',(-260.909689484712,113.464793580191,290.573593133701));
#17893=CARTESIAN_POINT('',(16.0838694668338,201.301935597134,290.573593133701));
#17894=CARTESIAN_POINT('',(15.0784816026316,200.967818784257,290.573593133701));
#17895=CARTESIAN_POINT('',(19.2205075843702,200.70865654923,290.573593133701));
#17896=CARTESIAN_POINT('Origin',(18.4341359467765,205.139414909555,290.573593133701));
#17897=CARTESIAN_POINT('Origin',(36.6954328642313,102.247359653123,290.573593133701));
#17898=CARTESIAN_POINT('',(68.8536755000203,196.935518525169,290.573593133701));
#17899=CARTESIAN_POINT('Origin',(36.6954328642313,102.247359653123,290.573593133701));
#17900=CARTESIAN_POINT('',(291.864989043215,121.19582713314,290.573593133701));
#17901=CARTESIAN_POINT('',(302.041252647846,117.739737607039,290.573593133701));
#17902=CARTESIAN_POINT('',(302.041252647846,106.992603302334,290.573593133701));
#17903=CARTESIAN_POINT('Origin',(287.041252647846,106.992603302334,290.573593133701));
#17904=CARTESIAN_POINT('',(302.041252647846,52.7397376070391,290.573593133701));
#17905=CARTESIAN_POINT('',(302.041252647846,37.7397376070391,290.573593133701));
#17906=CARTESIAN_POINT('Origin',(287.041252647846,52.7397376070391,290.573593133701));
#17907=CARTESIAN_POINT('Origin',(37.0412526478464,207.739737607039,295.073593133701));
#17908=CARTESIAN_POINT('',(-259.490535542311,109.194430353513,295.073593133701));
#17909=CARTESIAN_POINT('',(-283.689260493489,101.152558013242,295.073593133701));
#17910=CARTESIAN_POINT('',(37.0412526478464,207.739737607039,295.073593133701));
#17911=CARTESIAN_POINT('',(-259.490535542311,109.194430353513,290.573593133701));
#17912=CARTESIAN_POINT('',(-283.689260493489,101.152558013242,295.073593133701));
#17913=CARTESIAN_POINT('Origin',(-293.959747352154,53.2771177754925,305.073593133701));
#17914=CARTESIAN_POINT('',(173.041252647846,39.7397376070391,305.073593133701));
#17915=CARTESIAN_POINT('',(173.041252647846,53.2771177754925,305.073593133701));
#17916=CARTESIAN_POINT('',(173.041252647846,53.2771177754925,305.073593133701));
#17917=CARTESIAN_POINT('',(176.041252647846,39.7397376070391,305.073593133701));
#17918=CARTESIAN_POINT('',(-293.959747352154,39.7397376070391,305.073593133701));
#17919=CARTESIAN_POINT('',(176.041252647846,53.2771177754925,305.073593133701));
#17920=CARTESIAN_POINT('',(176.041252647846,53.2771177754925,305.073593133701));
#17921=CARTESIAN_POINT('',(-293.959747352154,53.2771177754925,305.073593133701));
#17922=CARTESIAN_POINT('Origin',(-293.959747352154,53.2771177754925,315.073593133701));
#17923=CARTESIAN_POINT('',(176.041252647846,62.8635864382735,312.227610249438));
#17924=CARTESIAN_POINT('Origin',(176.041252647846,53.2771177754925,315.073593133701));
#17925=CARTESIAN_POINT('',(173.041252647846,62.8635864382735,312.227610249438));
#17926=CARTESIAN_POINT('',(-293.959747352154,62.8635864382735,312.227610249438));
#17927=CARTESIAN_POINT('Origin',(173.041252647846,53.2771177754925,315.073593133701));
#17928=CARTESIAN_POINT('Origin',(-276.958747352154,52.7397376070391,295.073593133701));
#17929=CARTESIAN_POINT('',(81.7733034554153,36.7397376070391,295.073593133701));
#17930=CARTESIAN_POINT('Origin',(80.0412526478464,35.7397376070391,295.073593133701));
#17931=CARTESIAN_POINT('',(262.309201840278,36.7397376070391,295.073593133701));
#17932=CARTESIAN_POINT('',(-276.958747352154,36.7397376070391,295.073593133701));
#17933=CARTESIAN_POINT('',(264.041252647846,37.7397376070391,295.073593133701));
#17934=CARTESIAN_POINT('Origin',(264.041252647846,35.7397376070391,295.073593133701));
#17935=CARTESIAN_POINT('',(287.041252647846,37.7397376070391,295.073593133701));
#17936=CARTESIAN_POINT('',(-293.958747352154,37.7397376070391,295.073593133701));
#17937=CARTESIAN_POINT('',(302.041252647846,52.7397376070391,295.073593133701));
#17938=CARTESIAN_POINT('Origin',(287.041252647846,52.7397376070391,295.073593133701));
#17939=CARTESIAN_POINT('',(302.041252647846,106.992603302334,295.073593133701));
#17940=CARTESIAN_POINT('',(302.041252647846,37.7397376070391,295.073593133701));
#17941=CARTESIAN_POINT('',(291.864989043215,121.19582713314,295.073593133701));
#17942=CARTESIAN_POINT('Origin',(287.041252647846,106.992603302334,295.073593133701));
#17943=CARTESIAN_POINT('',(68.8536755000203,196.935518525169,295.073593133701));
#17944=CARTESIAN_POINT('',(302.041252647846,117.739737607039,295.073593133701));
#17945=CARTESIAN_POINT('',(24.6736703960697,201.522115896385,295.073593133701));
#17946=CARTESIAN_POINT('Origin',(36.6954328642313,102.247359653123,295.073593133701));
#17947=CARTESIAN_POINT('',(-254.589437230121,108.715645084056,295.073593133701));
#17948=CARTESIAN_POINT('',(-291.486115520766,96.4539090962283,295.073593133701));
#17949=CARTESIAN_POINT('',(-256.639326258033,114.883947522592,295.073593133701));
#17950=CARTESIAN_POINT('',(-240.062069061508,65.0014735948669,295.073593133701));
#17951=CARTESIAN_POINT('Origin',(-260.909689484712,113.464793580191,295.073593133701));
#17952=CARTESIAN_POINT('',(-293.958747352154,86.9180139243132,295.073593133701));
#17953=CARTESIAN_POINT('Origin',(-278.958747352154,86.9180139243132,295.073593133701));
#17954=CARTESIAN_POINT('',(-293.958747352154,52.7397376070391,295.073593133701));
#17955=CARTESIAN_POINT('',(-293.958747352154,97.7397376070391,295.073593133701));
#17956=CARTESIAN_POINT('Origin',(-278.958747352154,52.7397376070391,295.073593133701));
#17957=CARTESIAN_POINT('',(173.041252647846,82.7397376070391,295.073593133701));
#17958=CARTESIAN_POINT('',(173.041252647846,88.7397376070391,295.073593133701));
#17959=CARTESIAN_POINT('',(179.041252647847,88.7397376070391,295.073593133701));
#17960=CARTESIAN_POINT('Origin',(179.041252647847,82.7397376070391,295.073593133701));
#17961=CARTESIAN_POINT('',(232.990318796651,88.7397376070391,295.073593133701));
#17962=CARTESIAN_POINT('',(173.041252647846,88.7397376070391,295.073593133701));
#17963=CARTESIAN_POINT('',(239.041252647847,82.7397376070391,295.073593133701));
#17964=CARTESIAN_POINT('Origin',(232.990318796658,82.7397376070451,295.073593133701));
#17965=CARTESIAN_POINT('',(239.041252647847,88.7397376070391,295.073593133701));
#17966=CARTESIAN_POINT('',(82.0412526478464,37.7397376070391,295.073593133701));
#17967=CARTESIAN_POINT('Origin',(-293.958747352154,97.7397376070391,295.073593133701));
#17968=CARTESIAN_POINT('',(-293.958747352154,52.7397376070391,295.073593133701));
#17969=CARTESIAN_POINT('',(-293.958747352154,86.9180139243132,295.073593133701));
#17970=CARTESIAN_POINT('Origin',(-293.958747352154,37.7397376070391,295.073593133701));
#17971=CARTESIAN_POINT('',(264.041252647846,37.7397376070391,295.073593133701));
#17972=CARTESIAN_POINT('',(287.041252647846,37.7397376070391,295.073593133701));
#17973=CARTESIAN_POINT('Origin',(302.041252647846,37.7397376070391,295.073593133701));
#17974=CARTESIAN_POINT('',(302.041252647846,52.7397376070391,295.073593133701));
#17975=CARTESIAN_POINT('',(302.041252647846,106.992603302334,295.073593133701));
#17976=CARTESIAN_POINT('Origin',(302.041252647846,117.739737607039,295.073593133701));
#17977=CARTESIAN_POINT('',(291.864989043215,121.19582713314,295.073593133701));
#17978=CARTESIAN_POINT('',(68.8536755000203,196.935518525169,295.073593133701));
#17979=CARTESIAN_POINT('Origin',(-276.958747352154,52.7397376070391,307.323593133701));
#17980=CARTESIAN_POINT('Origin',(173.041252647846,88.7397376070391,339.073593133701));
#17981=CARTESIAN_POINT('',(173.041252647846,82.7397376070391,339.073593133701));
#17982=CARTESIAN_POINT('',(173.041252647846,70.8334876070391,339.073593133701));
#17983=CARTESIAN_POINT('',(173.041252647846,88.7397376070391,339.073593133701));
#17984=CARTESIAN_POINT('',(173.041252647846,82.7397376070391,295.073593133701));
#17985=CARTESIAN_POINT('Origin',(173.041252647846,39.7397376070391,303.073593133701));
#17986=CARTESIAN_POINT('',(173.041252647846,79.7397376070394,369.073593133702));
#17987=CARTESIAN_POINT('Origin',(203.041252647846,88.7397376070391,339.073593133701));
#17988=CARTESIAN_POINT('',(232.788727075195,82.7397376070391,342.95789039244));
#17989=CARTESIAN_POINT('',(232.788727075195,71.9866383557274,342.95789039244));
#17990=CARTESIAN_POINT('',(232.788727075195,88.7397376070391,342.95789039244));
#17991=CARTESIAN_POINT('Origin',(203.041252647846,82.7397376070391,339.073593133701));
#17992=CARTESIAN_POINT('Origin',(203.041252647846,70.8334876070392,339.073593133701));
#17993=CARTESIAN_POINT('Origin',(239.041252647847,88.7397376070391,295.073593133701));
#17994=CARTESIAN_POINT('',(232.788727075195,82.7397376070391,342.95789039244));
#17995=CARTESIAN_POINT('',(236.80135487697,62.8635864382735,312.227610249438));
#17996=CARTESIAN_POINT('',(221.30495438235,98.0959760916413,430.905133292361));
#17997=CARTESIAN_POINT('',(237.735495660568,53.2771177754925,305.073593133701));
#17998=CARTESIAN_POINT('Origin',(236.42973867329,53.2771177754957,315.073593133697));
#17999=CARTESIAN_POINT('',(237.735495660568,39.7397376070391,305.073593133701));
#18000=CARTESIAN_POINT('',(237.735495660568,53.2771177754925,305.073593133701));
#18001=CARTESIAN_POINT('Origin',(237.996647058023,39.7397376070351,303.073593133704));
#18002=CARTESIAN_POINT('Origin',(203.041252647846,88.7397376070391,339.073593133701));
#18003=CARTESIAN_POINT('',(179.041252647846,88.7397376070391,339.073593133701));
#18004=CARTESIAN_POINT('',(226.839232189725,88.7397376070391,342.181030940692));
#18005=CARTESIAN_POINT('Origin',(203.041252647846,88.7397376070391,339.073593133701));
#18006=CARTESIAN_POINT('',(233.091757762377,88.7397376070391,294.296733681953));
#18007=CARTESIAN_POINT('',(179.041252647846,88.7397376070391,339.073593133701));
#18008=CARTESIAN_POINT('Origin',(-293.959747352154,53.2771177754925,305.073593133701));
#18009=CARTESIAN_POINT('',(234.71002873497,53.2771177754925,305.073593133701));
#18010=CARTESIAN_POINT('',(234.71002873497,39.7397376070391,305.073593133701));
#18011=CARTESIAN_POINT('',(234.71002873497,53.2771177754925,305.073593133701));
#18012=CARTESIAN_POINT('',(-293.959747352154,39.7397376070391,305.073593133701));
#18013=CARTESIAN_POINT('',(-293.959747352154,53.2771177754925,305.073593133701));
#18014=CARTESIAN_POINT('Origin',(-293.959747352154,53.2771177754925,315.073593133701));
#18015=CARTESIAN_POINT('',(233.775887951372,62.8635864382735,312.227610249438));
#18016=CARTESIAN_POINT('',(-293.959747352154,62.8635864382735,312.227610249438));
#18017=CARTESIAN_POINT('Origin',(233.404271747692,53.2771177754959,315.073593133697));
#18018=CARTESIAN_POINT('Origin',(-293.959747352154,79.7397376070391,369.073593133701));
#18019=CARTESIAN_POINT('',(176.041252647846,70.8334876070391,339.073593133701));
#18020=CARTESIAN_POINT('',(176.041252647846,79.7397376070391,369.073593133701));
#18021=CARTESIAN_POINT('',(229.81397963246,71.8713232808586,342.569460666566));
#18022=CARTESIAN_POINT('Origin',(203.041252647846,70.8334876070391,339.073593133701));
#18023=CARTESIAN_POINT('',(218.326162231599,97.9898570057982,430.547679529521));
#18024=CARTESIAN_POINT('Origin',(203.041252647846,85.7397376070391,339.073593133701));
#18025=CARTESIAN_POINT('',(231.506382410955,85.7397376070391,298.714756191828));
#18026=CARTESIAN_POINT('',(225.847649708814,85.7397376070391,342.051554365401));
#18027=CARTESIAN_POINT('',(225.847649708814,85.7397376070391,342.051554365401));
#18028=CARTESIAN_POINT('',(180.041252647846,85.7397376070391,339.073593133701));
#18029=CARTESIAN_POINT('Origin',(203.041252647846,85.7397376070391,339.073593133701));
#18030=CARTESIAN_POINT('',(180.041252647846,85.7397376070391,299.047792462302));
#18031=CARTESIAN_POINT('',(180.041252647846,85.7397376070391,339.073593133701));
#18032=CARTESIAN_POINT('',(202.781289236061,85.7397376070391,298.900639292561));
#18033=CARTESIAN_POINT('Origin',(176.041252647846,182.009983898606,305.073593133701));
#18034=CARTESIAN_POINT('Origin',(176.041252647846,39.7397376070391,303.073593133701));
#18035=CARTESIAN_POINT('',(176.041252647846,81.7397376070391,299.047792462302));
#18036=CARTESIAN_POINT('',(176.041252647846,85.7397376070391,299.047792462302));
#18037=CARTESIAN_POINT('',(176.041252647846,81.7397376070391,339.073593133701));
#18038=CARTESIAN_POINT('',(176.041252647846,81.7397376070391,305.073593133701));
#18039=CARTESIAN_POINT('',(176.041252647846,182.009983898606,339.073593133701));
#18040=CARTESIAN_POINT('Origin',(203.041252647846,182.009983898606,339.073593133701));
#18041=CARTESIAN_POINT('',(229.81397963246,81.7397376070391,342.569460666566));
#18042=CARTESIAN_POINT('Origin',(203.041252647846,81.7397376070391,339.073593133701));
#18043=CARTESIAN_POINT('',(229.81397963246,182.009983898606,342.569460666566));
#18044=CARTESIAN_POINT('Origin',(233.826607434235,182.009983898606,311.839180523564));
#18045=CARTESIAN_POINT('Origin',(234.971180132426,39.7397376070352,303.073593133704));
#18046=CARTESIAN_POINT('',(235.472712334602,81.7397376070391,299.232662492993));
#18047=CARTESIAN_POINT('',(233.826607434235,81.7397376070391,311.839180523564));
#18048=CARTESIAN_POINT('',(235.472712334602,37.7397376070391,299.232662492993));
#18049=CARTESIAN_POINT('Origin',(176.041252647846,182.009983898606,295.073593133701));
#18050=CARTESIAN_POINT('',(180.015368768859,37.7397376070391,295.047876210078));
#18051=CARTESIAN_POINT('',(231.480498531968,37.7397376070391,294.714839939603));
#18052=CARTESIAN_POINT('',(176.041252647846,37.7397376070391,295.073593133701));
#18053=CARTESIAN_POINT('',(231.480498531968,81.7397376070391,294.714839939603));
#18054=CARTESIAN_POINT('',(231.480498531968,85.7397376070391,294.714839939603));
#18055=CARTESIAN_POINT('',(180.015368768859,81.7397376070391,295.047876210078));
#18056=CARTESIAN_POINT('',(176.041252647846,81.7397376070391,295.073593133701));
#18057=CARTESIAN_POINT('',(180.015368768859,37.7397376070391,295.047876210078));
#18058=CARTESIAN_POINT('Origin',(36.6954328642313,102.247359653123,295.073593133701));
#18059=CARTESIAN_POINT('',(19.2205075843702,200.70865654923,291.2246677273));
#18060=CARTESIAN_POINT('',(19.2205075843702,200.70865654923,295.073593133701));
#18061=CARTESIAN_POINT('',(14.7441480327787,199.808320566024,295.756533633647));
#18062=CARTESIAN_POINT('Origin',(36.6954313613018,102.247367094447,305.692991109406));
#18063=CARTESIAN_POINT('Ctrl Pts',(14.7441480327787,199.808320566023,295.756533633647));
#18064=CARTESIAN_POINT('Ctrl Pts',(14.7577154236595,199.811373238515,295.754954515747));
#18065=CARTESIAN_POINT('Ctrl Pts',(14.7712835464547,199.814423097892,295.753376761062));
#18066=CARTESIAN_POINT('Ctrl Pts',(18.1382702274613,200.570522874585,295.362462384317));
#18067=CARTESIAN_POINT('Ctrl Pts',(21.5391004439812,201.142532437006,295.073593133701));
#18068=CARTESIAN_POINT('Ctrl Pts',(24.6736703960694,201.522115896385,295.073593133701));
#18069=CARTESIAN_POINT('Origin',(36.6954328642313,102.247359653123,290.573593133701));
#18070=CARTESIAN_POINT('Origin',(287.041252647846,52.7397376070391,295.073593133701));
#18071=CARTESIAN_POINT('Origin',(287.041252647846,106.992603302334,295.073593133701));
#18072=CARTESIAN_POINT('Origin',(-278.958747352154,52.7397376070391,295.073593133701));
#18073=CARTESIAN_POINT('Origin',(-278.958747352154,86.9180139243132,295.073593133701));
#18074=CARTESIAN_POINT('Origin',(-293.536004548678,102.622211534764,315.573593133701));
#18075=CARTESIAN_POINT('',(-216.352417040558,128.272346356194,315.573593133701));
#18076=CARTESIAN_POINT('',(-26.4698977858668,191.375298374369,315.573593133701));
#18077=CARTESIAN_POINT('',(-293.536004548678,102.622211534764,315.573593133701));
#18078=CARTESIAN_POINT('',(-214.933263098157,124.001983129515,315.573593133701));
#18079=CARTESIAN_POINT('',(-216.352417040558,128.272346356194,315.573593133701));
#18080=CARTESIAN_POINT('',(-25.0507438434661,187.104935147691,315.573593133701));
#18081=CARTESIAN_POINT('',(-292.116850606278,98.3518483080855,315.573593133701));
#18082=CARTESIAN_POINT('',(-26.4698977858668,191.375298374369,315.573593133701));
#18083=CARTESIAN_POINT('Origin',(-292.116850606278,98.3518483080855,253.073593133701));
#18084=CARTESIAN_POINT('',(-253.322233103775,111.244319381425,297.073593133701));
#18085=CARTESIAN_POINT('',(-250.497473803234,112.183061142934,300.050252536588));
#18086=CARTESIAN_POINT('',(-293.596873185455,97.8599979041293,254.633203230727));
#18087=CARTESIAN_POINT('',(13.3382261621522,199.862598895781,297.073593133701));
#18088=CARTESIAN_POINT('',(-292.116850606278,98.3518483080855,297.073593133701));
#18089=CARTESIAN_POINT('',(10.5134668616108,198.923857134272,300.050252536588));
#18090=CARTESIAN_POINT('',(-118.511980891635,156.045309542559,436.013983036675));
#18091=CARTESIAN_POINT('Origin',(-25.050743843466,187.104935147691,262.573593133701));
#18092=CARTESIAN_POINT('Origin',(-214.933263098157,124.001983129515,262.573593133701));
#18093=CARTESIAN_POINT('Origin',(-295.016027127856,102.130361130808,254.633203230727));
#18094=CARTESIAN_POINT('',(-251.916627745634,116.453424369613,300.050252536588));
#18095=CARTESIAN_POINT('',(-295.016027127856,102.130361130808,254.633203230727));
#18096=CARTESIAN_POINT('Origin',(-252.691498018264,109.346380169568,297.0735931337));
#18097=CARTESIAN_POINT('',(-251.916627745634,116.453424369613,300.050252536588));
#18098=CARTESIAN_POINT('Origin',(13.8170114316087,204.763697207971,253.073593133701));
#18099=CARTESIAN_POINT('',(13.8170114316087,204.763697207971,295.073593133701));
#18100=CARTESIAN_POINT('',(14.1637727200978,203.720260967154,295.073593133701));
#18101=CARTESIAN_POINT('',(13.8170114316087,204.763697207971,295.073593133701));
#18102=CARTESIAN_POINT('',(14.1637727200979,203.720260967154,291.819075083293));
#18103=CARTESIAN_POINT('',(14.1637727200979,203.720260967154,253.073593133701));
#18104=CARTESIAN_POINT('',(13.8170114316087,204.763697207971,294.573593133701));
#18105=CARTESIAN_POINT('Origin',(15.0784816026316,200.967818784257,294.573593133701));
#18106=CARTESIAN_POINT('',(13.8170114316087,204.763697207971,253.073593133701));
#18107=CARTESIAN_POINT('Origin',(-119.931134834035,160.315672769238,436.013983036675));
#18108=CARTESIAN_POINT('',(9.09431291921015,203.194220360951,300.050252536588));
#18109=CARTESIAN_POINT('',(-119.931134834035,160.315672769238,436.013983036675));
#18110=CARTESIAN_POINT('',(9.09431291921009,203.194220360951,300.050252536588));
#18111=CARTESIAN_POINT('Origin',(13.9689612476602,197.964659683904,297.073593133711));
#18112=CARTESIAN_POINT('Origin',(18.434135946777,205.139414909556,290.5735931337));
#18113=CARTESIAN_POINT('Origin',(-293.536004548678,102.622211534764,253.073593133701));
#18114=CARTESIAN_POINT('',(-256.639326258033,114.883947522592,294.573593133701));
#18115=CARTESIAN_POINT('',(-256.639326258033,114.883947522592,294.573593133701));
#18116=CARTESIAN_POINT('',(-256.639326258033,114.883947522592,253.073593133701));
#18117=CARTESIAN_POINT('Origin',(-216.352417040558,128.272346356194,262.573593133701));
#18118=CARTESIAN_POINT('Origin',(-26.4698977858667,191.375298374369,262.573593133701));
#18119=CARTESIAN_POINT('Origin',(277.041252647846,78.7397376070391,283.573593133701));
#18120=CARTESIAN_POINT('Origin',(37.0412526478464,187.739737607039,273.573593133701));
#18121=CARTESIAN_POINT('Origin',(11.0412526478464,112.739737607039,285.573593133701));
#18122=CARTESIAN_POINT('Origin',(-293.958747352154,97.7397376070391,211.073593133701));
#18123=CARTESIAN_POINT('',(-293.958747352154,52.7397376070391,215.573593133701));
#18124=CARTESIAN_POINT('',(-293.958747352154,52.7397376070391,211.073593133701));
#18125=CARTESIAN_POINT('',(-293.958747352154,86.9180139243132,215.573593133701));
#18126=CARTESIAN_POINT('',(-293.958747352154,97.7397376070391,215.573593133701));
#18127=CARTESIAN_POINT('',(-293.958747352154,86.9180139243132,211.073593133701));
#18128=CARTESIAN_POINT('Origin',(37.0412526478464,207.739737607039,211.073593133701));
#18129=CARTESIAN_POINT('',(-283.689260493489,101.152558013242,215.573593133701));
#18130=CARTESIAN_POINT('',(37.0412526478464,207.739737607039,215.573593133701));
#18131=CARTESIAN_POINT('',(-283.689260493489,101.152558013242,211.073593133701));
#18132=CARTESIAN_POINT('Origin',(302.041252647846,117.739737607039,211.073593133701));
#18133=CARTESIAN_POINT('',(291.864989043215,121.19582713314,215.573593133701));
#18134=CARTESIAN_POINT('',(302.041252647846,117.739737607039,215.573593133701));
#18135=CARTESIAN_POINT('',(291.864989043215,121.19582713314,211.073593133701));
#18136=CARTESIAN_POINT('Origin',(302.041252647846,37.7397376070391,211.073593133701));
#18137=CARTESIAN_POINT('',(302.041252647846,52.7397376070391,215.573593133701));
#18138=CARTESIAN_POINT('',(302.041252647846,106.992603302334,215.573593133701));
#18139=CARTESIAN_POINT('',(302.041252647846,37.7397376070391,215.573593133701));
#18140=CARTESIAN_POINT('',(302.041252647846,52.7397376070391,211.073593133701));
#18141=CARTESIAN_POINT('',(302.041252647846,106.992603302334,211.073593133701));
#18142=CARTESIAN_POINT('Origin',(-276.958747352154,52.7397376070391,215.573593133701));
#18143=CARTESIAN_POINT('',(81.7733034554153,36.7397376070391,215.573593133701));
#18144=CARTESIAN_POINT('Origin',(80.0412526478464,35.7397376070391,215.573593133701));
#18145=CARTESIAN_POINT('',(262.309201840278,36.7397376070391,215.573593133701));
#18146=CARTESIAN_POINT('',(-276.958747352154,36.7397376070391,215.573593133701));
#18147=CARTESIAN_POINT('Origin',(264.041252647846,35.7397376070391,215.573593133701));
#18148=CARTESIAN_POINT('Origin',(287.041252647846,52.7397376070391,215.573593133701));
#18149=CARTESIAN_POINT('Origin',(287.041252647846,106.992603302334,215.573593133701));
#18150=CARTESIAN_POINT('',(16.0838694668338,201.301935597134,215.573593133701));
#18151=CARTESIAN_POINT('Origin',(18.4341359467765,205.139414909555,215.573593133701));
#18152=CARTESIAN_POINT('',(-255.37785608701,111.088069098878,215.573593133701));
#18153=CARTESIAN_POINT('Origin',(-278.958747352154,86.9180139243132,215.573593133701));
#18154=CARTESIAN_POINT('Origin',(-278.958747352154,52.7397376070391,215.573593133701));
#18155=CARTESIAN_POINT('Origin',(-276.958747352154,52.7397376070391,198.823593133701));
#18156=CARTESIAN_POINT('Origin',(203.041252647846,88.7397376070391,167.073593133701));
#18157=CARTESIAN_POINT('',(226.839232189725,88.7397376070391,163.966155326709));
#18158=CARTESIAN_POINT('',(179.041252647846,88.7397376070391,167.073593133701));
#18159=CARTESIAN_POINT('Origin',(176.041252647846,182.009983898606,211.073593133701));
#18160=CARTESIAN_POINT('',(180.041252647846,85.7397376070391,211.099477554629));
#18161=CARTESIAN_POINT('',(176.041252647846,85.7397376070391,211.073593133701));
#18162=CARTESIAN_POINT('',(180.015368768859,37.7397376070391,211.099310057324));
#18163=CARTESIAN_POINT('',(176.041252647846,37.7397376070391,211.073593133701));
#18164=CARTESIAN_POINT('',(180.015368768859,85.7396538592634,211.099310057324));
#18165=CARTESIAN_POINT('',(180.015368768859,85.7397376070391,211.099310057324));
#18166=CARTESIAN_POINT('Origin',(180.041272326363,81.733660909987,211.099477683049));
#18167=CARTESIAN_POINT('Origin',(176.041252647846,182.009983898606,167.073593133701));
#18168=CARTESIAN_POINT('Origin',(176.041252647846,39.7397376070391,203.073593133701));
#18169=CARTESIAN_POINT('',(176.041252647846,81.7397376070391,207.0993938051));
#18170=CARTESIAN_POINT('',(176.041252647846,81.7397376070391,211.073593133701));
#18171=CARTESIAN_POINT('',(176.041252647846,37.7397376070391,207.0993938051));
#18172=CARTESIAN_POINT('Origin',(234.760748217833,182.009983898606,201.462022859575));
#18173=CARTESIAN_POINT('Origin',(234.971180132426,39.7397376070408,203.073593133702));
#18174=CARTESIAN_POINT('',(229.81397963246,81.7397376070391,163.577725600835));
#18175=CARTESIAN_POINT('Origin',(203.041252647846,85.7397376070391,339.073593133701));
#18176=CARTESIAN_POINT('',(232.100175281465,85.7397376070391,211.97992916074));
#18177=CARTESIAN_POINT('',(180.041252647846,85.7397376070391,167.073593133701));
#18178=CARTESIAN_POINT('Origin',(287.041252647846,52.7397376070391,211.073593133701));
#18179=CARTESIAN_POINT('Origin',(287.041252647846,106.992603302334,211.073593133701));
#18180=CARTESIAN_POINT('Origin',(-278.958747352154,52.7397376070391,211.073593133701));
#18181=CARTESIAN_POINT('Origin',(-278.958747352154,86.9180139243132,211.073593133701));
#18182=CARTESIAN_POINT('Origin',(13.8170114316087,204.763697207971,253.073593133701));
#18183=CARTESIAN_POINT('',(13.8170114316087,204.763697207971,211.573593133701));
#18184=CARTESIAN_POINT('',(14.1637727200979,203.720260967154,214.328111184109));
#18185=CARTESIAN_POINT('Origin',(15.0784816026316,200.967818784257,211.573593133701));
#18186=CARTESIAN_POINT('',(14.1637727200978,203.720260967154,211.073593133701));
#18187=CARTESIAN_POINT('',(14.1637727200979,203.720260967154,211.073593133701));
#18188=CARTESIAN_POINT('',(13.8170114316087,204.763697207971,211.073593133701));
#18189=CARTESIAN_POINT('',(13.8170114316087,204.763697207971,211.073593133701));
#18190=CARTESIAN_POINT('',(13.8170114316087,204.763697207971,253.073593133701));
#18191=CARTESIAN_POINT('Origin',(-119.931134834035,160.315672769238,70.1332032307269));
#18192=CARTESIAN_POINT('',(9.09431291921009,203.194220360951,206.096933730814));
#18193=CARTESIAN_POINT('',(9.09431291921003,203.194220360951,206.096933730813));
#18194=CARTESIAN_POINT('',(-119.931134834035,160.315672769238,70.1332032307269));
#18195=CARTESIAN_POINT('Origin',(18.4341359467765,205.139414909555,215.573593133701));
#18196=CARTESIAN_POINT('Origin',(13.9689612476676,197.964659683866,209.073593133684));
#18197=CARTESIAN_POINT('Origin',(-293.536004548678,102.622211534764,190.573593133701));
#18198=CARTESIAN_POINT('',(-216.352417040558,128.272346356194,190.573593133701));
#18199=CARTESIAN_POINT('',(-216.352417040558,128.272346356194,190.573593133701));
#18200=CARTESIAN_POINT('',(-26.4698977858668,191.375298374369,190.573593133701));
#18201=CARTESIAN_POINT('',(-293.536004548678,102.622211534764,190.573593133701));
#18202=CARTESIAN_POINT('',(-26.4698977858668,191.375298374369,190.573593133701));
#18203=CARTESIAN_POINT('Origin',(-295.016027127856,102.130361130808,251.513983036674));
#18204=CARTESIAN_POINT('',(-251.916627745634,116.453424369613,206.096933730814));
#18205=CARTESIAN_POINT('',(-295.016027127856,102.130361130808,251.513983036674));
#18206=CARTESIAN_POINT('',(-251.916627745634,116.453424369613,206.096933730814));
#18207=CARTESIAN_POINT('Origin',(-252.691498018267,109.346380169569,209.073593133703));
#18208=CARTESIAN_POINT('Origin',(-293.536004548678,102.622211534764,253.073593133701));
#18209=CARTESIAN_POINT('',(13.8170114316088,204.763697207971,211.573593133701));
#18210=CARTESIAN_POINT('Origin',(-26.4698977858668,191.375298374369,243.573593133701));
#18211=CARTESIAN_POINT('Origin',(-216.352417040558,128.272346356194,243.573593133701));
#18212=CARTESIAN_POINT('Origin',(277.041252647846,78.7397376070391,222.573593133701));
#18213=CARTESIAN_POINT('Origin',(37.0412526478464,187.739737607039,232.573593133701));
#18214=CARTESIAN_POINT('Origin',(11.0412526478464,112.739737607039,220.573593133701));
#18215=CARTESIAN_POINT('Origin',(82.0412526478464,37.7397376070391,290.573593133701));
#18216=CARTESIAN_POINT('Origin',(231.506382410955,37.7397376070391,298.714756191828));
#18217=CARTESIAN_POINT('Origin',(180.041252647846,37.7397376070391,299.047792462302));
#18218=CARTESIAN_POINT('Origin',(82.0412526478464,34.7397376070391,290.573593133701));
#18219=CARTESIAN_POINT('',(262.041252647846,34.7397376070391,217.573593133701));
#18220=CARTESIAN_POINT('',(262.041252647846,34.7397376070391,288.573593133701));
#18221=CARTESIAN_POINT('',(262.041252647846,34.7397376070391,290.573593133701));
#18222=CARTESIAN_POINT('',(82.0412526478464,34.7397376070391,217.573593133701));
#18223=CARTESIAN_POINT('',(82.0412526478464,34.7397376070391,217.573593133701));
#18224=CARTESIAN_POINT('',(82.0412526478464,34.7397376070391,288.573593133701));
#18225=CARTESIAN_POINT('',(82.0412526478464,34.7397376070391,290.573593133701));
#18226=CARTESIAN_POINT('',(82.0412526478464,34.7397376070391,288.573593133701));
#18227=CARTESIAN_POINT('Origin',(82.0412526478464,37.7397376070391,215.573593133701));
#18228=CARTESIAN_POINT('Origin',(180.041252647846,37.7397376070391,207.0993938051));
#18229=CARTESIAN_POINT('Origin',(82.0412526478464,30.2397376070391,295.073593133701));
#18230=CARTESIAN_POINT('',(262.041252647846,30.2397376070391,288.573593133701));
#18231=CARTESIAN_POINT('',(262.041252647846,30.2397376070391,217.573593133701));
#18232=CARTESIAN_POINT('',(262.041252647846,30.2397376070391,295.073593133701));
#18233=CARTESIAN_POINT('',(82.0412526478464,30.2397376070391,288.573593133701));
#18234=CARTESIAN_POINT('',(82.0412526478464,30.2397376070391,288.573593133701));
#18235=CARTESIAN_POINT('',(82.0412526478464,30.2397376070391,217.573593133701));
#18236=CARTESIAN_POINT('',(82.0412526478464,30.2397376070391,295.073593133701));
#18237=CARTESIAN_POINT('',(82.0412526478464,30.2397376070391,217.573593133701));
#18238=CARTESIAN_POINT('Origin',(82.0412526478464,52.7397376070391,253.073593133701));
#18239=CARTESIAN_POINT('',(82.0412526478464,35.7397376070391,294.996209423033));
#18240=CARTESIAN_POINT('Origin',(82.0412526478464,36.7397376070391,288.573593133701));
#18241=CARTESIAN_POINT('',(82.0412526478464,35.7397376070391,290.30564394127));
#18242=CARTESIAN_POINT('',(82.0412526478464,35.7397376070391,290.573593133701));
#18243=CARTESIAN_POINT('Origin',(82.0412526478464,36.7397376070391,288.573593133701));
#18244=CARTESIAN_POINT('',(82.0412526478464,35.7397376070391,215.841542326132));
#18245=CARTESIAN_POINT('Origin',(82.0412526478464,36.7397376070391,217.573593133701));
#18246=CARTESIAN_POINT('',(82.0412526478464,35.7397376070391,211.150976844368));
#18247=CARTESIAN_POINT('',(82.0412526478464,35.7397376070391,253.073593133701));
#18248=CARTESIAN_POINT('Origin',(82.0412526478464,36.7397376070391,217.573593133701));
#18249=CARTESIAN_POINT('Origin',(262.041252647846,52.7397376070391,253.073593133701));
#18250=CARTESIAN_POINT('',(262.041252647846,35.7397376070391,290.30564394127));
#18251=CARTESIAN_POINT('',(262.041252647846,35.7397376070391,294.996209423033));
#18252=CARTESIAN_POINT('',(262.041252647846,35.7397376070391,253.073593133701));
#18253=CARTESIAN_POINT('Origin',(262.041252647846,36.7397376070391,288.573593133701));
#18254=CARTESIAN_POINT('',(262.041252647846,35.7397376070391,211.150976844368));
#18255=CARTESIAN_POINT('Origin',(262.041252647846,36.7397376070391,217.573593133701));
#18256=CARTESIAN_POINT('',(262.041252647846,35.7397376070391,215.841542326132));
#18257=CARTESIAN_POINT('',(262.041252647846,35.7397376070391,215.573593133701));
#18258=CARTESIAN_POINT('Origin',(262.041252647846,36.7397376070391,217.573593133701));
#18259=CARTESIAN_POINT('Origin',(262.041252647846,36.7397376070391,288.573593133701));
#18260=CARTESIAN_POINT('Origin',(-216.352417040558,128.272346356194,243.573593133701));
#18261=CARTESIAN_POINT('Origin',(-26.4698977858668,191.375298374369,243.573593133701));
#18262=CARTESIAN_POINT('Origin',(-216.352417040558,128.272346356194,262.573593133701));
#18263=CARTESIAN_POINT('Origin',(-26.4698977858667,191.375298374369,262.573593133701));
#18264=CARTESIAN_POINT('Origin',(180.041252647846,182.009983898606,207.0993938051));
#18265=CARTESIAN_POINT('Origin',(180.041252647849,81.7397376070372,207.099393805098));
#18266=CARTESIAN_POINT('Origin',(180.041252647846,81.7397376070391,339.073593133701));
#18267=CARTESIAN_POINT('Origin',(247.930162753351,81.7397376070391,333.212192331543));
#18268=CARTESIAN_POINT('Origin',(180.041252647846,182.009983898606,299.047792462302));
#18269=CARTESIAN_POINT('Origin',(180.041252647846,81.7397376070391,299.047792462302));
#18270=CARTESIAN_POINT('Origin',(231.506382410955,182.009983898606,298.714756191828));
#18271=CARTESIAN_POINT('Origin',(231.506382410955,81.7397376070391,298.714756191828));
#18272=CARTESIAN_POINT('Origin',(176.067136526834,81.7397376070391,299.073509385925));
#18273=CARTESIAN_POINT('Origin',(180.041252647846,81.7397376070391,299.047792462302));
#18274=CARTESIAN_POINT('Origin',(231.506382410955,81.7397376070391,298.714756191828));
#18275=CARTESIAN_POINT('Origin',(180.041252647846,81.7397376070391,299.047792462302));
#18276=CARTESIAN_POINT('Origin',(180.041252647846,81.7397376070391,299.047792462302));
#18277=CARTESIAN_POINT('Origin',(231.506382410955,81.7397376070391,298.714756191828));
#18278=CARTESIAN_POINT('Origin',(231.506382410955,81.7397376070391,298.714756191828));
#18279=CARTESIAN_POINT('Origin',(180.041252647846,81.7397376070391,305.073593133701));
#18280=CARTESIAN_POINT('Origin',(180.041252647846,81.7397376070391,339.073593133701));
#18281=CARTESIAN_POINT('Origin',(229.860277510589,81.7397376070391,311.321274222398));
#18282=CARTESIAN_POINT('Origin',(225.847649708814,81.7397376070391,342.051554365401));
#18283=CARTESIAN_POINT('Origin',(203.041252647846,81.7397376070391,339.073593133701));
#18284=CARTESIAN_POINT('Origin',(-292.274534377656,98.8263331110498,211.573593133701));
#18285=CARTESIAN_POINT('Ctrl Pts',(16.0838694668338,201.301935597134,215.573593133701));
#18286=CARTESIAN_POINT('Ctrl Pts',(15.9358379539975,201.392597584931,215.573593133701));
#18287=CARTESIAN_POINT('Ctrl Pts',(15.7937040698879,201.491453806169,215.566973449043));
#18288=CARTESIAN_POINT('Ctrl Pts',(15.4044650646298,201.796472278373,215.524024592965));
#18289=CARTESIAN_POINT('Ctrl Pts',(15.1550912170556,202.039779480087,215.462189646269));
#18290=CARTESIAN_POINT('Ctrl Pts',(14.7363053891028,202.553699758439,215.248657229881));
#18291=CARTESIAN_POINT('Ctrl Pts',(14.5662939349351,202.823424001646,215.095998687681));
#18292=CARTESIAN_POINT('Ctrl Pts',(14.3222646393754,203.293147538743,214.753756991984));
#18293=CARTESIAN_POINT('Ctrl Pts',(14.2316333870611,203.51606205111,214.554691098869));
#18294=CARTESIAN_POINT('Ctrl Pts',(14.1637727200979,203.720260967154,214.328111184109));
#18295=CARTESIAN_POINT('Origin',(-292.274534377656,98.8263331110498,294.573593133701));
#18296=CARTESIAN_POINT('Ctrl Pts',(14.1637727200979,203.720260967154,291.819075083293));
#18297=CARTESIAN_POINT('Ctrl Pts',(14.2316333870611,203.51606205111,291.592495168533));
#18298=CARTESIAN_POINT('Ctrl Pts',(14.3222646393754,203.293147538743,291.393429275417));
#18299=CARTESIAN_POINT('Ctrl Pts',(14.5662939349351,202.823424001646,291.05118757972));
#18300=CARTESIAN_POINT('Ctrl Pts',(14.7363053891028,202.553699758439,290.898529037521));
#18301=CARTESIAN_POINT('Ctrl Pts',(15.1550912170556,202.039779480087,290.684996621132));
#18302=CARTESIAN_POINT('Ctrl Pts',(15.4044650646298,201.796472278373,290.623161674437));
#18303=CARTESIAN_POINT('Ctrl Pts',(15.7937040698879,201.491453806169,290.580212818359));
#18304=CARTESIAN_POINT('Ctrl Pts',(15.9358379539975,201.392597584931,290.573593133701));
#18305=CARTESIAN_POINT('Ctrl Pts',(16.0838694668338,201.301935597134,290.573593133701));
#18306=CARTESIAN_POINT('Ctrl Pts',(-257.691868353317,110.319062001313,290.573593133701));
#18307=CARTESIAN_POINT('Ctrl Pts',(-257.226722972947,110.794866944168,290.573593133701));
#18308=CARTESIAN_POINT('Ctrl Pts',(-256.875952954917,111.37569206742,290.610062934072));
#18309=CARTESIAN_POINT('Ctrl Pts',(-256.575993830868,112.221556348799,290.839959190792));
#18310=CARTESIAN_POINT('Ctrl Pts',(-256.503984375586,112.507585568265,290.942908485374));
#18311=CARTESIAN_POINT('Ctrl Pts',(-256.419927726647,113.054277491751,291.217469046592));
#18312=CARTESIAN_POINT('Ctrl Pts',(-256.406892655266,113.314450931809,291.389750558212));
#18313=CARTESIAN_POINT('Ctrl Pts',(-256.416576787744,113.953138581935,291.926969681713));
#18314=CARTESIAN_POINT('Ctrl Pts',(-256.482778257329,114.307185871813,292.394274351607));
#18315=CARTESIAN_POINT('Ctrl Pts',(-256.596967428487,114.771542993549,293.443240125));
#18316=CARTESIAN_POINT('Ctrl Pts',(-256.639326258033,114.883947522592,294.024578076468));
#18317=CARTESIAN_POINT('Ctrl Pts',(-256.639326258033,114.883947522592,294.573593133701));
#18318=CARTESIAN_POINT('Origin',(-276.958747352154,36.7397376070391,217.573593133701));
#18319=CARTESIAN_POINT('Ctrl Pts',(262.041252647846,35.7397376070391,215.841542326132));
#18320=CARTESIAN_POINT('Ctrl Pts',(262.041252647846,35.8848665867868,215.757752070607));
#18321=CARTESIAN_POINT('Ctrl Pts',(262.058271315733,36.0525570221457,215.687285114485));
#18322=CARTESIAN_POINT('Ctrl Pts',(262.141705134945,36.3891914211257,215.596855314572));
#18323=CARTESIAN_POINT('Ctrl Pts',(262.208584003366,36.5579076658357,215.576473827892));
#18324=CARTESIAN_POINT('Ctrl Pts',(262.295835118638,36.7163102167537,215.573696499521));
#18325=CARTESIAN_POINT('Ctrl Pts',(262.302427956789,36.728004896672,215.573593133701));
#18326=CARTESIAN_POINT('Ctrl Pts',(262.309201840278,36.7397376070391,215.573593133701));
#18327=CARTESIAN_POINT('Ctrl Pts',(81.7733034554153,36.7397376070391,215.573593133701));
#18328=CARTESIAN_POINT('Ctrl Pts',(81.7800773389041,36.728004896672,215.573593133701));
#18329=CARTESIAN_POINT('Ctrl Pts',(81.7866701770546,36.7163102167537,215.573696499521));
#18330=CARTESIAN_POINT('Ctrl Pts',(81.8739212923264,36.5579076658357,215.576473827892));
#18331=CARTESIAN_POINT('Ctrl Pts',(81.9408001607482,36.3891914211257,215.596855314572));
#18332=CARTESIAN_POINT('Ctrl Pts',(82.0242339799602,36.0525570221457,215.687285114485));
#18333=CARTESIAN_POINT('Ctrl Pts',(82.0412526478464,35.8848665867869,215.757752070607));
#18334=CARTESIAN_POINT('Ctrl Pts',(82.0412526478464,35.7397376070391,215.841542326132));
#18335=CARTESIAN_POINT('Origin',(82.0412526478464,36.7397376070391,288.573593133701));
#18336=CARTESIAN_POINT('Ctrl Pts',(82.0412526478464,35.7397376070391,290.30564394127));
#18337=CARTESIAN_POINT('Ctrl Pts',(82.0412526478464,35.8848665867869,290.389434196794));
#18338=CARTESIAN_POINT('Ctrl Pts',(82.0242339799602,36.0525570221457,290.459901152916));
#18339=CARTESIAN_POINT('Ctrl Pts',(81.9408001607482,36.3891914211257,290.55033095283));
#18340=CARTESIAN_POINT('Ctrl Pts',(81.8739212923264,36.5579076658357,290.57071243951));
#18341=CARTESIAN_POINT('Ctrl Pts',(81.7866701770546,36.7163102167537,290.57348976788));
#18342=CARTESIAN_POINT('Ctrl Pts',(81.7800773389041,36.728004896672,290.573593133701));
#18343=CARTESIAN_POINT('Ctrl Pts',(81.7733034554153,36.7397376070391,290.573593133701));
#18344=CARTESIAN_POINT('Ctrl Pts',(262.309201840278,36.7397376070391,290.573593133701));
#18345=CARTESIAN_POINT('Ctrl Pts',(262.302427956789,36.728004896672,290.573593133701));
#18346=CARTESIAN_POINT('Ctrl Pts',(262.295835118638,36.7163102167537,290.57348976788));
#18347=CARTESIAN_POINT('Ctrl Pts',(262.208584003366,36.5579076658357,290.57071243951));
#18348=CARTESIAN_POINT('Ctrl Pts',(262.141705134945,36.3891914211257,290.55033095283));
#18349=CARTESIAN_POINT('Ctrl Pts',(262.058271315733,36.0525570221457,290.459901152916));
#18350=CARTESIAN_POINT('Ctrl Pts',(262.041252647846,35.8848665867869,290.389434196794));
#18351=CARTESIAN_POINT('Ctrl Pts',(262.041252647846,35.7397376070391,290.30564394127));
#18352=CARTESIAN_POINT('Origin',(-293.958747352154,39.7397376070391,203.073593133701));
#18353=CARTESIAN_POINT('Origin',(-293.958747352154,39.7397376070391,203.073593133701));
#18354=CARTESIAN_POINT('Origin',(-291.486115520766,96.4539090962284,297.073593133701));
#18355=CARTESIAN_POINT('Origin',(-291.486115520766,96.4539090962284,209.073593133701));
#18356=CARTESIAN_POINT('Origin',(-293.959747352154,39.7397376070391,303.073593133701));
#18357=CARTESIAN_POINT('Origin',(-293.959747352154,39.7397376070391,303.073593133701));
#18358=CARTESIAN_POINT('Ctrl Pts',(33.5102687927929,200.251018647718,288.573578335645));
#18359=CARTESIAN_POINT('Ctrl Pts',(33.5107199010858,200.251129484782,290.575563586967));
#18360=CARTESIAN_POINT('Ctrl Pts',(32.9669590743211,202.177851622247,290.573593109838));
#18361=CARTESIAN_POINT('Ctrl Pts',(34.0920283034919,200.415203421348,288.573424517396));
#18362=CARTESIAN_POINT('Ctrl Pts',(34.0347498209467,200.399019089839,290.421586252515));
#18363=CARTESIAN_POINT('Ctrl Pts',(33.6443849144762,202.203125958631,290.573595060035));
#18364=CARTESIAN_POINT('Ctrl Pts',(34.6840502924345,200.538691146292,288.592342587767));
#18365=CARTESIAN_POINT('Ctrl Pts',(34.6313932427609,200.529729997912,290.326885010332));
#18366=CARTESIAN_POINT('Ctrl Pts',(34.328746338229,202.221780639051,290.573596347446));
#18367=CARTESIAN_POINT('Ctrl Pts',(35.5864205375463,200.661622866077,288.615706152486));
#18368=CARTESIAN_POINT('Ctrl Pts',(35.5496884468174,200.657467722248,290.241178426705));
#18369=CARTESIAN_POINT('Ctrl Pts',(35.3681885540774,202.239169784339,290.573597581329));
#18370=CARTESIAN_POINT('Ctrl Pts',(35.8896886164042,200.692165047495,288.622846769446));
#18371=CARTESIAN_POINT('Ctrl Pts',(35.8596462675485,200.689666471269,290.22149043692));
#18372=CARTESIAN_POINT('Ctrl Pts',(35.716916186513,202.243194275642,290.573597875706));
#18373=CARTESIAN_POINT('Ctrl Pts',(36.4932960055171,200.731705119721,288.632640790062));
#18374=CARTESIAN_POINT('Ctrl Pts',(36.4764185460958,200.731103852825,290.196200221347));
#18375=CARTESIAN_POINT('Ctrl Pts',(36.4104416468938,202.247575398223,290.573598260089));
#18376=CARTESIAN_POINT('Ctrl Pts',(36.794514742425,200.740872444726,288.635321175873));
#18377=CARTESIAN_POINT('Ctrl Pts',(36.7867685126652,200.740894737748,290.190242235453));
#18378=CARTESIAN_POINT('Ctrl Pts',(36.7562545492582,202.247957465234,290.573598351964));
#18379=CARTESIAN_POINT('Ctrl Pts',(37.6964382193845,200.737132673354,288.635298337225));
#18380=CARTESIAN_POINT('Ctrl Pts',(37.7120443346043,200.737055769037,290.190295279034));
#18381=CARTESIAN_POINT('Ctrl Pts',(37.7918313998826,202.243752845543,290.573598351148));
#18382=CARTESIAN_POINT('Ctrl Pts',(38.2954125861561,200.693134716753,288.623593248778));
#18383=CARTESIAN_POINT('Ctrl Pts',(38.3371819114897,200.688812702912,290.213470083842));
#18384=CARTESIAN_POINT('Ctrl Pts',(38.4797294520679,202.233829054631,290.573597994748));
#18385=CARTESIAN_POINT('Ctrl Pts',(39.4912382499762,200.521128467222,288.592642194352));
#18386=CARTESIAN_POINT('Ctrl Pts',(39.5436846822378,200.511806765647,290.325533254215));
#18387=CARTESIAN_POINT('Ctrl Pts',(39.8584875384269,202.199733195285,290.573596366356));
#18388=CARTESIAN_POINT('Ctrl Pts',(40.0910570919123,200.391481338985,288.573422072675));
#18389=CARTESIAN_POINT('Ctrl Pts',(40.1485301709568,200.374739220995,290.421119323041));
#18390=CARTESIAN_POINT('Ctrl Pts',(40.5529097792499,202.175269274473,290.57359506633));
#18391=CARTESIAN_POINT('Ctrl Pts',(40.6733598348467,200.222036935988,288.573578350593));
#18392=CARTESIAN_POINT('Ctrl Pts',(40.6729077590008,200.222151960831,290.57556998517));
#18393=CARTESIAN_POINT('Ctrl Pts',(41.2322427580752,202.144417149988,290.57359310976));
#18394=CARTESIAN_POINT('Ctrl Pts',(40.6733364731919,200.222043778143,217.573607931757));
#18395=CARTESIAN_POINT('Ctrl Pts',(40.672886276363,200.222158261008,215.571622680597));
#18396=CARTESIAN_POINT('Ctrl Pts',(41.2322163763533,202.144418355354,215.573593157564));
#18397=CARTESIAN_POINT('Ctrl Pts',(40.0929242452915,200.390929578713,217.573761750004));
#18398=CARTESIAN_POINT('Ctrl Pts',(40.1500699231558,200.374282397278,215.725600014994));
#18399=CARTESIAN_POINT('Ctrl Pts',(40.5550171724534,202.175172199407,215.573591207367));
#18400=CARTESIAN_POINT('Ctrl Pts',(39.5019206382725,200.51920268524,217.554843679621));
#18401=CARTESIAN_POINT('Ctrl Pts',(39.5545034696285,200.509815837693,215.820301257091));
#18402=CARTESIAN_POINT('Ctrl Pts',(39.8708290592947,202.199362712531,215.573589919956));
#18403=CARTESIAN_POINT('Ctrl Pts',(38.6005744329249,200.649430503753,217.531480114922));
#18404=CARTESIAN_POINT('Ctrl Pts',(38.6372717067624,200.644978335475,215.906007840698));
#18405=CARTESIAN_POINT('Ctrl Pts',(38.8315615356453,202.225160314443,215.573588686073));
#18406=CARTESIAN_POINT('Ctrl Pts',(38.2975633626732,200.682425106419,217.524339497957));
#18407=CARTESIAN_POINT('Ctrl Pts',(38.3275845150866,200.679683571143,215.925695830483));
#18408=CARTESIAN_POINT('Ctrl Pts',(38.4828778729045,202.232005859847,215.573588391695));
#18409=CARTESIAN_POINT('Ctrl Pts',(37.6942956028995,200.726847032593,217.514545477341));
#18410=CARTESIAN_POINT('Ctrl Pts',(37.7111676458084,200.726109247728,215.950986046056));
#18411=CARTESIAN_POINT('Ctrl Pts',(37.7894105505436,202.241997418763,215.573588007313));
#18412=CARTESIAN_POINT('Ctrl Pts',(37.3931608862198,200.738450899264,217.511865091529));
#18413=CARTESIAN_POINT('Ctrl Pts',(37.4009070428415,200.73841052502,215.956944031954));
#18414=CARTESIAN_POINT('Ctrl Pts',(37.4436120554966,202.245177079077,215.573587915438));
#18415=CARTESIAN_POINT('Ctrl Pts',(36.4912366693717,200.742007757534,217.511887930177));
#18416=CARTESIAN_POINT('Ctrl Pts',(36.4756304426942,200.742057108271,215.95689098836));
#18417=CARTESIAN_POINT('Ctrl Pts',(36.4080350780731,202.249350352081,215.573587916253));
#18418=CARTESIAN_POINT('Ctrl Pts',(35.89192596265,200.702856907713,217.523593018625));
#18419=CARTESIAN_POINT('Ctrl Pts',(35.850123039343,200.698872946658,215.933716183589));
#18420=CARTESIAN_POINT('Ctrl Pts',(35.7200792538628,202.244991940212,215.573588272656));
#18421=CARTESIAN_POINT('Ctrl Pts',(34.6947479110263,200.540530445424,217.554544073045));
#18422=CARTESIAN_POINT('Ctrl Pts',(34.6422277830206,200.531633337413,215.821653013178));
#18423=CARTESIAN_POINT('Ctrl Pts',(34.3410904528754,202.22205126753,215.573589901044));
#18424=CARTESIAN_POINT('Ctrl Pts',(34.0938998602774,200.41574005857,217.573764194676));
#18425=CARTESIAN_POINT('Ctrl Pts',(34.0362932192499,200.399463442246,215.726066944493));
#18426=CARTESIAN_POINT('Ctrl Pts',(33.6464930249784,202.203205981858,215.573591201072));
#18427=CARTESIAN_POINT('Ctrl Pts',(33.5102453777233,200.251011995113,217.573607916811));
#18428=CARTESIAN_POINT('Ctrl Pts',(33.5106983692828,200.251123358914,215.571616282394));
#18429=CARTESIAN_POINT('Ctrl Pts',(32.9669326850786,202.177850630394,215.573593157641));
#18430=CARTESIAN_POINT('Origin',(179.041252647846,82.7397376070391,167.073593133701));
#18431=CARTESIAN_POINT('Origin',(226.839232189725,82.7397376070391,163.966155326709));
#18432=CARTESIAN_POINT('Origin',(179.041252647846,82.7397376070391,339.073593133701));
#18433=CARTESIAN_POINT('Origin',(179.041252647846,82.7397376070391,339.073593133701));
#18434=CARTESIAN_POINT('Origin',(203.041252647846,82.7397376070391,339.073593133701));
#18435=CARTESIAN_POINT('Origin',(226.839232189725,82.7397376070391,342.181030940692));
#18436=CARTESIAN_POINT('Origin',(233.091757762377,82.7397376070391,294.296733681953));
#18437=CARTESIAN_POINT('Origin',(80.0412526478464,35.7397376070391,295.073593133701));
#18438=CARTESIAN_POINT('Ctrl Pts',(82.0412526478464,35.7397376070391,294.996209423033));
#18439=CARTESIAN_POINT('Ctrl Pts',(82.0412526478464,35.9880846920539,295.034877011727));
#18440=CARTESIAN_POINT('Ctrl Pts',(81.9920100122073,36.2549156690397,295.0601656977));
#18441=CARTESIAN_POINT('Ctrl Pts',(81.8568715998261,36.5831910390556,295.072227252638));
#18442=CARTESIAN_POINT('Ctrl Pts',(81.8175214272437,36.6631498332247,295.073593133701));
#18443=CARTESIAN_POINT('Ctrl Pts',(81.7733034554153,36.7397376070391,295.073593133701));
#18444=CARTESIAN_POINT('Origin',(80.0412526478464,35.7397376070391,211.073593133701));
#18445=CARTESIAN_POINT('Ctrl Pts',(81.7733034554153,36.7397376070391,211.073593133701));
#18446=CARTESIAN_POINT('Ctrl Pts',(81.8175214272437,36.6631498332247,211.073593133701));
#18447=CARTESIAN_POINT('Ctrl Pts',(81.8568715998261,36.5831910390556,211.074959014763));
#18448=CARTESIAN_POINT('Ctrl Pts',(81.9920100122073,36.2549156690397,211.087020569701));
#18449=CARTESIAN_POINT('Ctrl Pts',(82.0412526478464,35.9880846920539,211.112309255674));
#18450=CARTESIAN_POINT('Ctrl Pts',(82.0412526478464,35.7397376070391,211.150976844368));
#18451=CARTESIAN_POINT('Origin',(264.041252647846,35.7397376070391,253.073593133701));
#18452=CARTESIAN_POINT('Ctrl Pts',(262.041252647846,35.7397376070391,211.150976844368));
#18453=CARTESIAN_POINT('Ctrl Pts',(262.041252647846,35.9880846920539,211.112309255674));
#18454=CARTESIAN_POINT('Ctrl Pts',(262.090495283485,36.2549156690397,211.087020569701));
#18455=CARTESIAN_POINT('Ctrl Pts',(262.225633695867,36.5831910390556,211.074959014763));
#18456=CARTESIAN_POINT('Ctrl Pts',(262.264983868449,36.6631498332246,211.073593133701));
#18457=CARTESIAN_POINT('Ctrl Pts',(262.309201840278,36.7397376070391,211.073593133701));
#18458=CARTESIAN_POINT('Origin',(264.041252647846,35.7397376070391,253.073593133701));
#18459=CARTESIAN_POINT('Ctrl Pts',(262.309201840278,36.7397376070391,295.073593133701));
#18460=CARTESIAN_POINT('Ctrl Pts',(262.264983868449,36.6631498332247,295.073593133701));
#18461=CARTESIAN_POINT('Ctrl Pts',(262.225633695867,36.5831910390556,295.072227252638));
#18462=CARTESIAN_POINT('Ctrl Pts',(262.090495283485,36.2549156690397,295.0601656977));
#18463=CARTESIAN_POINT('Ctrl Pts',(262.041252647846,35.9880846920539,295.034877011727));
#18464=CARTESIAN_POINT('Ctrl Pts',(262.041252647846,35.7397376070391,294.996209423033));
#18465=CARTESIAN_POINT('Origin',(-260.909689484712,113.464793580191,253.073593133701));
#18466=CARTESIAN_POINT('Origin',(18.4341359467765,205.139414909555,211.073593133701));
#18467=CARTESIAN_POINT('Origin',(18.4341359467765,205.139414909555,295.073593133701));
#18468=CARTESIAN_POINT('Origin',(-276.958747352154,36.7397376070391,288.573593133701));
#18469=CARTESIAN_POINT('Origin',(82.0412526478464,36.7397376070391,217.573593133701));
#18470=CARTESIAN_POINT('',(0.,0.,0.));
#18471=CARTESIAN_POINT('',(0.,0.,0.));
#18472=CARTESIAN_POINT('Origin',(46.4876128454249,129.573387746387,272.073593133701));
#18473=CARTESIAN_POINT('',(30.1995535821213,114.050851696014,234.073593133701));
#18474=CARTESIAN_POINT('',(49.4633471679037,107.271033493035,234.073593133701));
#18475=CARTESIAN_POINT('Origin',(46.4876128454249,129.573387746387,234.073593133701));
#18476=CARTESIAN_POINT('',(49.4633471679037,107.271033493035,239.073593133701));
#18477=CARTESIAN_POINT('',(49.4633471679037,107.271033493035,272.073593133701));
#18478=CARTESIAN_POINT('',(30.1995535821213,114.050851696014,239.073593133701));
#18479=CARTESIAN_POINT('Origin',(46.4876128454249,129.573387746387,239.073593133701));
#18480=CARTESIAN_POINT('',(30.1995535821213,114.050851696014,272.073593133701));
#18481=CARTESIAN_POINT('Origin',(-232.939627118345,176.278148255689,234.073593133701));
#18482=CARTESIAN_POINT('',(28.8182642450608,115.50026192826,234.073593133701));
#18483=CARTESIAN_POINT('',(-55.5594395041075,204.039211666113,234.073593133701));
#18484=CARTESIAN_POINT('',(-4.90646155624503,132.218021461828,234.073593133701));
#18485=CARTESIAN_POINT('Origin',(-10.9969917319035,77.5562849162387,234.073593133701));
#18486=CARTESIAN_POINT('',(-192.605807708699,153.131892918133,234.073593133701));
#18487=CARTESIAN_POINT('',(-213.799107820696,155.493296744853,234.073593133701));
#18488=CARTESIAN_POINT('',(-227.957953056828,160.0244433382,234.073593133701));
#18489=CARTESIAN_POINT('',(77.1627332513468,100.535558183572,234.073593133701));
#18490=CARTESIAN_POINT('',(-227.713166902474,192.45480160587,234.073593133701));
#18491=CARTESIAN_POINT('Origin',(-232.939627118345,176.278148255689,234.073593133701));
#18492=CARTESIAN_POINT('',(-177.982268468343,201.373715997924,234.073593133701));
#18493=CARTESIAN_POINT('',(-235.587533185649,191.042585036641,234.073593133701));
#18494=CARTESIAN_POINT('',(-177.989077795293,205.373710202053,234.073593133701));
#18495=CARTESIAN_POINT('',(-177.982268468343,201.373715997924,234.073593133701));
#18496=CARTESIAN_POINT('',(-177.41038412351,208.374699678994,234.073593133701));
#18497=CARTESIAN_POINT('Origin',(-169.989089387034,205.387328855953,234.073593133701));
#18498=CARTESIAN_POINT('',(48.4156221649759,208.759131013669,234.073593133701));
#18499=CARTESIAN_POINT('',(-232.99410509728,208.28007760959,234.073593133701));
#18500=CARTESIAN_POINT('',(61.4104021126536,188.99066912614,234.073593133701));
#18501=CARTESIAN_POINT('Origin',(31.8750805350466,183.730937259653,234.073593133701));
#18502=CARTESIAN_POINT('',(70.7697436798221,136.43453699661,234.073593133701));
#18503=CARTESIAN_POINT('',(56.9969630433931,213.773746568613,234.073593133701));
#18504=CARTESIAN_POINT('Origin',(46.1569756984829,132.05142710787,234.073593133701));
#18505=CARTESIAN_POINT('',(45.0412410561795,187.753356260924,234.073593133701));
#18506=CARTESIAN_POINT('Origin',(37.0412526479213,187.739737607024,234.073593133701));
#18507=CARTESIAN_POINT('',(54.6251789940657,132.579591357641,234.073593133701));
#18508=CARTESIAN_POINT('Origin',(43.6251949327106,132.560865708529,234.073593133701));
#18509=CARTESIAN_POINT('Origin',(15.,130.,272.073593133701));
#18510=CARTESIAN_POINT('',(28.8182642450609,115.50026192826,239.073593133701));
#18511=CARTESIAN_POINT('',(10.0701475636351,135.172977429866,239.073593133701));
#18512=CARTESIAN_POINT('',(28.8182642450609,115.50026192826,272.073593133701));
#18513=CARTESIAN_POINT('Origin',(46.4876128454249,129.573387746387,272.073593133701));
#18514=CARTESIAN_POINT('',(30.1995535821213,114.050851696014,267.073593133701));
#18515=CARTESIAN_POINT('',(49.4633471679037,107.271033493035,267.073593133701));
#18516=CARTESIAN_POINT('Origin',(46.4876128454249,129.573387746387,267.073593133701));
#18517=CARTESIAN_POINT('',(49.4633471679037,107.271033493035,272.073593133701));
#18518=CARTESIAN_POINT('',(49.4633471679037,107.271033493035,272.073593133701));
#18519=CARTESIAN_POINT('',(30.1995535821213,114.050851696014,272.073593133701));
#18520=CARTESIAN_POINT('Origin',(46.4876128454249,129.573387746387,272.073593133701));
#18521=CARTESIAN_POINT('',(30.1995535821213,114.050851696014,272.073593133701));
#18522=CARTESIAN_POINT('Origin',(76.9784177883129,208.807754437623,267.073593133701));
#18523=CARTESIAN_POINT('',(28.8182642450609,115.50026192826,267.073593133701));
#18524=CARTESIAN_POINT('',(10.0701475636351,135.172977429866,267.073593133701));
#18525=CARTESIAN_POINT('',(-4.90646155624504,132.218021461828,267.073593133701));
#18526=CARTESIAN_POINT('Origin',(-10.9969917319035,77.5562849162387,267.073593133701));
#18527=CARTESIAN_POINT('',(-192.605807708699,153.131892918133,267.073593133701));
#18528=CARTESIAN_POINT('',(-62.5303325346189,138.638599131169,267.073593133701));
#18529=CARTESIAN_POINT('',(-235.81010437183,161.555364540059,267.073593133701));
#18530=CARTESIAN_POINT('',(77.1627332513468,100.535558183572,267.073593133701));
#18531=CARTESIAN_POINT('',(-235.587533185649,191.042585036641,267.073593133701));
#18532=CARTESIAN_POINT('Origin',(-232.939627118345,176.278148255689,267.073593133701));
#18533=CARTESIAN_POINT('',(-177.982268468343,201.373715997924,267.073593133701));
#18534=CARTESIAN_POINT('',(-235.587533185649,191.042585036641,267.073593133701));
#18535=CARTESIAN_POINT('',(-177.989077795293,205.373710202053,267.073593133701));
#18536=CARTESIAN_POINT('',(-177.982268468343,201.373715997924,267.073593133701));
#18537=CARTESIAN_POINT('',(-175.415302813384,211.265781701023,267.073593133701));
#18538=CARTESIAN_POINT('Origin',(-169.989089387034,205.387328855953,267.073593133701));
#18539=CARTESIAN_POINT('',(-175.406982357971,206.378107240404,267.073593133701));
#18540=CARTESIAN_POINT('',(-175.23725350376,106.674503914668,267.073593133701));
#18541=CARTESIAN_POINT('',(46.4190297263865,206.75572924813,267.073593133701));
#18542=CARTESIAN_POINT('',(46.4190297263865,206.75572924813,267.073593133701));
#18543=CARTESIAN_POINT('',(46.4135532795135,209.972751416803,267.073593133701));
#18544=CARTESIAN_POINT('',(46.5887585805977,107.052125922394,267.073593133701));
#18545=CARTESIAN_POINT('',(61.4104021126536,188.99066912614,267.073593133701));
#18546=CARTESIAN_POINT('Origin',(31.8750805350466,183.730937259653,267.073593133701));
#18547=CARTESIAN_POINT('',(70.7697436798221,136.43453699661,267.073593133701));
#18548=CARTESIAN_POINT('',(56.9969630433931,213.773746568613,267.073593133701));
#18549=CARTESIAN_POINT('Origin',(46.1569756984829,132.05142710787,267.073593133701));
#18550=CARTESIAN_POINT('',(54.6251789940657,132.579591357641,267.073593133701));
#18551=CARTESIAN_POINT('Origin',(43.6251949327106,132.560865708529,267.073593133701));
#18552=CARTESIAN_POINT('',(-224.939638710086,176.291766909589,267.073593133701));
#18553=CARTESIAN_POINT('Origin',(-232.939627118345,176.278148255689,267.073593133701));
#18554=CARTESIAN_POINT('',(45.0412410561795,187.753356260924,267.073593133701));
#18555=CARTESIAN_POINT('Origin',(37.0412526479213,187.739737607024,267.073593133701));
#18556=CARTESIAN_POINT('Origin',(15.,130.,272.073593133701));
#18557=CARTESIAN_POINT('',(28.8182642450608,115.50026192826,272.073593133701));
#18558=CARTESIAN_POINT('',(-55.5594395041075,204.039211666113,272.073593133701));
#18559=CARTESIAN_POINT('',(28.8182642450609,115.50026192826,272.073593133701));
#18560=CARTESIAN_POINT('Origin',(-10.9969917319035,77.5562849162387,272.073593133701));
#18561=CARTESIAN_POINT('',(-4.90646155624504,132.218021461828,239.073593133701));
#18562=CARTESIAN_POINT('Origin',(-10.9969917319035,77.5562849162387,239.073593133701));
#18563=CARTESIAN_POINT('',(-4.90646155624505,132.218021461828,272.073593133701));
#18564=CARTESIAN_POINT('Origin',(-192.605807708699,153.131892918133,272.073593133701));
#18565=CARTESIAN_POINT('',(-192.605807708699,153.131892918133,239.073593133701));
#18566=CARTESIAN_POINT('',(-62.5303325346189,138.638599131169,239.073593133701));
#18567=CARTESIAN_POINT('',(-192.605807708699,153.131892918133,272.073593133701));
#18568=CARTESIAN_POINT('Origin',(-10.9969917319035,77.5562849162387,272.073593133701));
#18569=CARTESIAN_POINT('',(-4.90646155624503,132.218021461828,272.073593133701));
#18570=CARTESIAN_POINT('Origin',(-10.9969917319035,77.5562849162387,272.073593133701));
#18571=CARTESIAN_POINT('',(-4.90646155624505,132.218021461828,272.073593133701));
#18572=CARTESIAN_POINT('Origin',(-192.605807708699,153.131892918133,272.073593133701));
#18573=CARTESIAN_POINT('',(-192.605807708699,153.131892918133,272.073593133701));
#18574=CARTESIAN_POINT('',(-213.799107820696,155.493296744853,272.073593133701));
#18575=CARTESIAN_POINT('',(-192.605807708699,153.131892918133,272.073593133701));
#18576=CARTESIAN_POINT('Origin',(77.1627332513468,100.535558183572,272.073593133701));
#18577=CARTESIAN_POINT('',(-227.957953056828,160.0244433382,272.073593133701));
#18578=CARTESIAN_POINT('',(77.1627332513468,100.535558183572,272.073593133701));
#18579=CARTESIAN_POINT('',(-235.81010437183,161.555364540059,274.073593133701));
#18580=CARTESIAN_POINT('Ctrl Pts',(-227.957953056828,160.0244433382,272.073593133701));
#18581=CARTESIAN_POINT('Ctrl Pts',(-228.546093465915,160.139112119509,272.073593133701));
#18582=CARTESIAN_POINT('Ctrl Pts',(-229.187572714652,160.264180287842,272.136134864339));
#18583=CARTESIAN_POINT('Ctrl Pts',(-230.458368646174,160.511945308759,272.351265898181));
#18584=CARTESIAN_POINT('Ctrl Pts',(-231.087933232071,160.63469049461,272.502332384129));
#18585=CARTESIAN_POINT('Ctrl Pts',(-232.977506438015,161.003097516761,273.025168777333));
#18586=CARTESIAN_POINT('Ctrl Pts',(-234.523328491993,161.304483934547,273.594881913422));
#18587=CARTESIAN_POINT('Ctrl Pts',(-235.81010437183,161.555364540059,274.073593133701));
#18588=CARTESIAN_POINT('',(-235.81010437183,161.555364540059,272.073593133701));
#18589=CARTESIAN_POINT('Origin',(-232.939627118345,176.278148255689,272.073593133701));
#18590=CARTESIAN_POINT('',(70.7697436798221,136.43453699661,272.073593133701));
#18591=CARTESIAN_POINT('Origin',(46.1569756984829,132.05142710787,272.073593133701));
#18592=CARTESIAN_POINT('',(61.4104021126536,188.99066912614,272.073593133701));
#18593=CARTESIAN_POINT('',(56.9969630433931,213.773746568613,272.073593133701));
#18594=CARTESIAN_POINT('',(48.4156221649759,208.759131013669,272.073593133701));
#18595=CARTESIAN_POINT('Origin',(31.8750805350466,183.730937259653,272.073593133701));
#18596=CARTESIAN_POINT('',(-177.41038412351,208.374699678994,272.073593133701));
#18597=CARTESIAN_POINT('',(-169.994196382247,208.38732450905,272.073593133701));
#18598=CARTESIAN_POINT('',(-177.989077795293,205.373710202053,272.073593133701));
#18599=CARTESIAN_POINT('Origin',(-169.989089387034,205.387328855953,272.073593133701));
#18600=CARTESIAN_POINT('',(-177.982268468343,201.373715997924,272.073593133701));
#18601=CARTESIAN_POINT('',(-177.982268468343,201.373715997924,272.073593133701));
#18602=CARTESIAN_POINT('',(-227.713166902474,192.45480160587,272.073593133701));
#18603=CARTESIAN_POINT('',(-235.587533185649,191.042585036641,272.073593133701));
#18604=CARTESIAN_POINT('Origin',(-232.939627118345,176.278148255689,272.073593133701));
#18605=CARTESIAN_POINT('',(54.6251789940657,132.579591357641,272.073593133701));
#18606=CARTESIAN_POINT('Origin',(43.6251949327106,132.560865708529,272.073593133701));
#18607=CARTESIAN_POINT('',(45.0412410561795,187.753356260924,272.073593133701));
#18608=CARTESIAN_POINT('Origin',(37.0412526479213,187.739737607024,272.073593133701));
#18609=CARTESIAN_POINT('Origin',(77.1627332513468,100.535558183572,272.073593133701));
#18610=CARTESIAN_POINT('',(-235.81010437183,161.555364540059,239.073593133701));
#18611=CARTESIAN_POINT('',(77.1627332513468,100.535558183572,239.073593133701));
#18612=CARTESIAN_POINT('',(-235.81010437183,161.555364540059,232.073593133701));
#18613=CARTESIAN_POINT('',(-235.81010437183,161.555364540059,272.073593133701));
#18614=CARTESIAN_POINT('Ctrl Pts',(-235.81010437183,161.555364540059,232.073593133701));
#18615=CARTESIAN_POINT('Ctrl Pts',(-233.401640601645,161.085790266491,232.969598917216));
#18616=CARTESIAN_POINT('Ctrl Pts',(-230.521958535878,160.524343326381,234.073593133701));
#18617=CARTESIAN_POINT('Ctrl Pts',(-227.957953056828,160.0244433382,234.073593133701));
#18618=CARTESIAN_POINT('Origin',(-232.939627118345,176.278148255689,276.073593133701));
#18619=CARTESIAN_POINT('',(-217.93964885286,176.303683231751,275.773593133701));
#18620=CARTESIAN_POINT('Origin',(-232.939627118345,176.278148255689,275.773593133701));
#18621=CARTESIAN_POINT('',(-218.23964841817,176.30317253223,276.073593133701));
#18622=CARTESIAN_POINT('',(-218.23964841817,176.30317253223,276.073593133701));
#18623=CARTESIAN_POINT('Origin',(-232.939627118345,176.278148255689,276.073593133701));
#18624=CARTESIAN_POINT('Origin',(-232.939627118345,176.278148255689,230.373593133701));
#18625=CARTESIAN_POINT('',(-217.939648852861,176.303683231751,230.373593133701));
#18626=CARTESIAN_POINT('',(-247.939605383829,176.252613279627,230.373593133701));
#18627=CARTESIAN_POINT('Origin',(-232.939627118345,176.278148255689,230.373593133701));
#18628=CARTESIAN_POINT('Origin',(-232.939627118345,176.278148255689,230.373593133701));
#18629=CARTESIAN_POINT('',(-247.639605818519,176.253123979149,230.073593133701));
#18630=CARTESIAN_POINT('',(-247.939605383829,176.252613279627,230.373593133701));
#18631=CARTESIAN_POINT('Origin',(-232.939627118345,176.278148255689,230.073593133701));
#18632=CARTESIAN_POINT('Origin',(-232.939627118345,176.278148255689,274.073593133701));
#18633=CARTESIAN_POINT('',(-217.93964885286,176.303683231751,274.073593133701));
#18634=CARTESIAN_POINT('Origin',(-232.939627118345,176.278148255689,274.073593133701));
#18635=CARTESIAN_POINT('',(-235.587533185649,191.042585036641,274.073593133701));
#18636=CARTESIAN_POINT('Ctrl Pts',(-235.587533185649,191.042585036641,274.073593133701));
#18637=CARTESIAN_POINT('Ctrl Pts',(-233.172255493539,191.475749440407,273.177587350186));
#18638=CARTESIAN_POINT('Ctrl Pts',(-230.28442635535,191.993662884028,272.073593133701));
#18639=CARTESIAN_POINT('Ctrl Pts',(-227.713166902474,192.45480160587,272.073593133701));
#18640=CARTESIAN_POINT('Origin',(-232.939627118345,176.278148255689,274.073593133701));
#18641=CARTESIAN_POINT('Origin',(-232.939627118345,176.278148255689,232.073593133701));
#18642=CARTESIAN_POINT('',(-217.93964885286,176.303683231751,232.073593133701));
#18643=CARTESIAN_POINT('Origin',(-232.939627118345,176.278148255689,232.073593133701));
#18644=CARTESIAN_POINT('',(-235.587533185649,191.042585036641,232.073593133701));
#18645=CARTESIAN_POINT('Origin',(-232.939627118345,176.278148255689,232.073593133701));
#18646=CARTESIAN_POINT('Ctrl Pts',(-227.713166902474,192.45480160587,234.073593133701));
#18647=CARTESIAN_POINT('Ctrl Pts',(-228.302971253065,192.349024017356,234.073593133701));
#18648=CARTESIAN_POINT('Ctrl Pts',(-228.946265347253,192.233653389927,234.011051403062));
#18649=CARTESIAN_POINT('Ctrl Pts',(-230.220656559869,192.005099583638,233.79592036922));
#18650=CARTESIAN_POINT('Ctrl Pts',(-230.852002282766,191.891871819177,233.644853883273));
#18651=CARTESIAN_POINT('Ctrl Pts',(-232.746921387808,191.552030356226,233.122017490068));
#18652=CARTESIAN_POINT('Ctrl Pts',(-234.297116814936,191.274012851197,232.552304353979));
#18653=CARTESIAN_POINT('Ctrl Pts',(-235.587533185649,191.042585036641,232.073593133701));
#18654=CARTESIAN_POINT('Origin',(43.6251949327106,132.560865708529,272.073593133701));
#18655=CARTESIAN_POINT('',(54.6251789940657,132.579591357641,272.073593133701));
#18656=CARTESIAN_POINT('Origin',(37.0412526479213,187.739737607024,272.073593133701));
#18657=CARTESIAN_POINT('',(45.0412410561795,187.753356260924,272.073593133701));
#18658=CARTESIAN_POINT('Origin',(-232.939627118345,176.278148255689,272.073593133701));
#18659=CARTESIAN_POINT('',(-224.939638710086,176.291766909589,276.073593133701));
#18660=CARTESIAN_POINT('Origin',(-232.939627118345,176.278148255689,276.073593133701));
#18661=CARTESIAN_POINT('',(-224.939638710086,176.291766909589,272.073593133701));
#18662=CARTESIAN_POINT('Origin',(-232.939627118345,176.278148255689,272.073593133701));
#18663=CARTESIAN_POINT('',(-217.93964885286,176.303683231751,272.073593133701));
#18664=CARTESIAN_POINT('',(-235.587533185649,191.042585036641,239.073593133701));
#18665=CARTESIAN_POINT('Origin',(-232.939627118345,176.278148255689,239.073593133701));
#18666=CARTESIAN_POINT('',(-235.587533185649,191.042585036641,272.073593133701));
#18667=CARTESIAN_POINT('Origin',(43.6251949327106,132.560865708529,272.073593133701));
#18668=CARTESIAN_POINT('',(54.6251789940657,132.579591357641,239.073593133701));
#18669=CARTESIAN_POINT('Origin',(43.6251949327106,132.560865708529,239.073593133701));
#18670=CARTESIAN_POINT('',(54.6251789940657,132.579591357641,272.073593133701));
#18671=CARTESIAN_POINT('Origin',(37.0412526479213,187.739737607024,272.073593133701));
#18672=CARTESIAN_POINT('',(45.0412410561795,187.753356260924,239.073593133701));
#18673=CARTESIAN_POINT('Origin',(37.0412526479213,187.739737607024,239.073593133701));
#18674=CARTESIAN_POINT('',(45.0412410561795,187.753356260924,272.073593133701));
#18675=CARTESIAN_POINT('Origin',(-232.939627118345,176.278148255689,272.073593133701));
#18676=CARTESIAN_POINT('',(-224.939638710086,176.291766909589,239.073593133701));
#18677=CARTESIAN_POINT('Origin',(-232.939627118345,176.278148255689,239.073593133701));
#18678=CARTESIAN_POINT('',(-224.939638710086,176.291766909589,230.073593133701));
#18679=CARTESIAN_POINT('',(-224.939638710086,176.291766909589,272.073593133701));
#18680=CARTESIAN_POINT('Origin',(-232.939627118345,176.278148255689,230.073593133701));
#18681=CARTESIAN_POINT('Origin',(-232.939627118345,176.278148255689,272.073593133701));
#18682=CARTESIAN_POINT('',(-217.93964885286,176.303683231751,272.073593133701));
#18683=CARTESIAN_POINT('',(-235.587533185649,191.042585036641,272.073593133701));
#18684=CARTESIAN_POINT('Origin',(76.9784177883129,208.807754437623,239.073593133701));
#18685=CARTESIAN_POINT('',(-175.410387021446,208.378104342469,241.073593133701));
#18686=CARTESIAN_POINT('',(-175.410387021446,208.378104342469,265.073593133701));
#18687=CARTESIAN_POINT('',(-175.410387021446,208.378104342469,239.073593133701));
#18688=CARTESIAN_POINT('',(46.4156250629116,208.755726350194,241.073593133701));
#18689=CARTESIAN_POINT('',(46.4156250629116,208.755726350194,241.073593133701));
#18690=CARTESIAN_POINT('',(46.4156250629116,208.755726350194,265.073593133701));
#18691=CARTESIAN_POINT('',(46.4156250629116,208.755726350194,239.073593133701));
#18692=CARTESIAN_POINT('',(-175.410387021446,208.378104342469,265.073593133701));
#18693=CARTESIAN_POINT('Origin',(31.8750805350466,183.730937259653,272.073593133701));
#18694=CARTESIAN_POINT('',(31.824010582923,213.730893790622,239.073593133701));
#18695=CARTESIAN_POINT('Ctrl Pts',(48.4156221649759,208.759131013669,234.073593133701));
#18696=CARTESIAN_POINT('Ctrl Pts',(47.1896385418122,209.56935461014,234.073593133701));
#18697=CARTESIAN_POINT('Ctrl Pts',(45.8893226556104,210.298387522342,234.266240084391));
#18698=CARTESIAN_POINT('Ctrl Pts',(43.182667391614,211.558385445743,234.877469643646));
#18699=CARTESIAN_POINT('Ctrl Pts',(41.7767242102558,212.088894220586,235.29874407437));
#18700=CARTESIAN_POINT('Ctrl Pts',(37.4929130147176,213.350222803775,236.749321829369));
#18701=CARTESIAN_POINT('Ctrl Pts',(34.5450346732006,213.735525883001,237.962738090941));
#18702=CARTESIAN_POINT('Ctrl Pts',(31.824010582923,213.730893790622,239.073593133701));
#18703=CARTESIAN_POINT('',(31.824010582923,213.730893790622,267.073593133701));
#18704=CARTESIAN_POINT('',(31.824010582923,213.730893790622,272.073593133701));
#18705=CARTESIAN_POINT('Ctrl Pts',(31.8240105829231,213.730893790622,267.073593133701));
#18706=CARTESIAN_POINT('Ctrl Pts',(33.2842831762373,213.733379662604,267.669747787341));
#18707=CARTESIAN_POINT('Ctrl Pts',(34.8844074857718,213.623034356201,268.324081712763));
#18708=CARTESIAN_POINT('Ctrl Pts',(38.067190631896,213.129088570913,269.562579881701));
#18709=CARTESIAN_POINT('Ctrl Pts',(39.6508266059049,212.744886046318,270.143991098496));
#18710=CARTESIAN_POINT('Ctrl Pts',(42.2750677822305,211.898355182682,270.994988064577));
#18711=CARTESIAN_POINT('Ctrl Pts',(43.5675862165289,211.393971522727,271.369518426275));
#18712=CARTESIAN_POINT('Ctrl Pts',(46.0918857841089,210.185438113252,271.910455807107));
#18713=CARTESIAN_POINT('Ctrl Pts',(47.3240128653335,209.480549796096,272.073593133701));
#18714=CARTESIAN_POINT('Ctrl Pts',(48.415622164976,208.759131013669,272.073593133701));
#18715=CARTESIAN_POINT('',(61.4104021126536,188.99066912614,272.073593133701));
#18716=CARTESIAN_POINT('',(46.4135532795135,209.972751416803,239.073593133701));
#18717=CARTESIAN_POINT('',(46.4135532795135,209.972751416803,272.073593133701));
#18718=CARTESIAN_POINT('',(61.4104021126536,188.99066912614,239.073593133701));
#18719=CARTESIAN_POINT('Origin',(31.8750805350466,183.730937259653,239.073593133701));
#18720=CARTESIAN_POINT('',(61.4104021126536,188.99066912614,272.073593133701));
#18721=CARTESIAN_POINT('Origin',(-169.989089387034,205.387328855953,272.073593133701));
#18722=CARTESIAN_POINT('',(-170.002708040934,213.387317264211,239.073593133701));
#18723=CARTESIAN_POINT('',(-170.002708040934,213.387317264211,267.073593133701));
#18724=CARTESIAN_POINT('',(-170.002708040934,213.387317264211,272.073593133701));
#18725=CARTESIAN_POINT('Ctrl Pts',(-170.002708040934,213.387317264211,239.073593133701));
#18726=CARTESIAN_POINT('Ctrl Pts',(-170.753749210153,213.38603874114,238.479842095552));
#18727=CARTESIAN_POINT('Ctrl Pts',(-171.571319487893,213.273469607744,237.832779229032));
#18728=CARTESIAN_POINT('Ctrl Pts',(-173.16290966802,212.777967370924,236.600716776795));
#18729=CARTESIAN_POINT('Ctrl Pts',(-173.937251007441,212.394457262387,236.016364655997));
#18730=CARTESIAN_POINT('Ctrl Pts',(-175.162834807223,211.526126218123,235.150121220116));
#18731=CARTESIAN_POINT('Ctrl Pts',(-175.728422301512,211.014823745933,234.774113289777));
#18732=CARTESIAN_POINT('Ctrl Pts',(-176.707530587388,209.799946719515,234.234922296038));
#18733=CARTESIAN_POINT('Ctrl Pts',(-177.120418024857,209.095040075002,234.073593133701));
#18734=CARTESIAN_POINT('Ctrl Pts',(-177.41038412351,208.374699678994,234.073593133701));
#18735=CARTESIAN_POINT('',(-177.989077795293,205.373710202053,239.073593133701));
#18736=CARTESIAN_POINT('',(-177.989077795293,205.373710202053,272.073593133701));
#18737=CARTESIAN_POINT('',(-175.415302813384,211.265781701023,239.073593133701));
#18738=CARTESIAN_POINT('Origin',(-169.989089387034,205.387328855953,239.073593133701));
#18739=CARTESIAN_POINT('',(-175.415302813384,211.265781701023,272.073593133701));
#18740=CARTESIAN_POINT('',(-177.989077795293,205.373710202053,272.073593133701));
#18741=CARTESIAN_POINT('Ctrl Pts',(-177.41038412351,208.374699678994,272.073593133701));
#18742=CARTESIAN_POINT('Ctrl Pts',(-177.148926429536,209.024218845859,272.073593133701));
#18743=CARTESIAN_POINT('Ctrl Pts',(-176.783223638279,209.670726923257,271.94133193636));
#18744=CARTESIAN_POINT('Ctrl Pts',(-175.919217012443,210.804093658125,271.487456150798));
#18745=CARTESIAN_POINT('Ctrl Pts',(-175.421532019632,211.292236733482,271.167874220512));
#18746=CARTESIAN_POINT('Ctrl Pts',(-174.223592818156,212.235297258746,270.34369109411));
#18747=CARTESIAN_POINT('Ctrl Pts',(-173.398721571726,212.680063455512,269.726299154576));
#18748=CARTESIAN_POINT('Ctrl Pts',(-171.69360491859,213.25525034828,268.411275830787));
#18749=CARTESIAN_POINT('Ctrl Pts',(-170.813019784585,213.385937842814,267.714201743102));
#18750=CARTESIAN_POINT('Ctrl Pts',(-170.002708040934,213.387317264211,267.073593133701));
#18751=CARTESIAN_POINT('Origin',(-177.982268468343,201.373715997924,272.073593133701));
#18752=CARTESIAN_POINT('',(-177.982268468343,201.373715997924,272.073593133701));
#18753=CARTESIAN_POINT('Origin',(56.9969630433931,213.773746568613,272.073593133701));
#18754=CARTESIAN_POINT('',(70.7697436798221,136.43453699661,239.073593133701));
#18755=CARTESIAN_POINT('',(56.9969630433931,213.773746568613,239.073593133701));
#18756=CARTESIAN_POINT('',(70.7697436798221,136.43453699661,272.073593133701));
#18757=CARTESIAN_POINT('Origin',(-235.587533185649,191.042585036641,272.073593133701));
#18758=CARTESIAN_POINT('',(-177.982268468343,201.373715997924,239.073593133701));
#18759=CARTESIAN_POINT('',(-235.587533185649,191.042585036641,239.073593133701));
#18760=CARTESIAN_POINT('',(-177.982268468343,201.373715997924,272.073593133701));
#18761=CARTESIAN_POINT('Origin',(56.9969630433931,213.773746568613,272.073593133701));
#18762=CARTESIAN_POINT('',(70.7697436798221,136.43453699661,272.073593133701));
#18763=CARTESIAN_POINT('Origin',(-178.002696449192,213.373698610312,272.073593133701));
#18764=CARTESIAN_POINT('',(-178.002696449192,213.373698610312,239.073593133701));
#18765=CARTESIAN_POINT('',(31.824010582923,213.730893790622,267.073593133701));
#18766=CARTESIAN_POINT('Origin',(-177.982268468343,201.373715997924,272.073593133701));
#18767=CARTESIAN_POINT('',(-177.982268468343,201.373715997924,239.073593133701));
#18768=CARTESIAN_POINT('Origin',(-235.587533185649,191.042585036641,272.073593133701));
#18769=CARTESIAN_POINT('Origin',(76.9784177883129,208.807754437623,239.073593133701));
#18770=CARTESIAN_POINT('Origin',(46.1569756984829,132.05142710787,239.073593133701));
#18771=CARTESIAN_POINT('',(46.4190297263865,206.75572924813,239.073593133701));
#18772=CARTESIAN_POINT('',(46.5887585805977,107.052125922394,239.073593133701));
#18773=CARTESIAN_POINT('',(-175.406982357971,206.378107240404,239.073593133701));
#18774=CARTESIAN_POINT('',(-175.406982357971,206.378107240404,239.073593133701));
#18775=CARTESIAN_POINT('',(-175.23725350376,106.674503914668,239.073593133701));
#18776=CARTESIAN_POINT('Origin',(-232.939627118345,176.278148255689,276.073593133701));
#18777=CARTESIAN_POINT('Origin',(-232.939627118345,176.278148255689,230.073593133701));
#18778=CARTESIAN_POINT('Origin',(46.1569756984829,132.05142710787,272.073593133701));
#18779=CARTESIAN_POINT('Origin',(46.1569756984829,132.05142710787,272.073593133701));
#18780=CARTESIAN_POINT('Origin',(-175.23725350376,106.674503914668,267.073593133701));
#18781=CARTESIAN_POINT('Origin',(-175.406982357971,206.378107240404,241.073593133701));
#18782=CARTESIAN_POINT('Origin',(-175.406982357971,206.378107240404,265.073593133701));
#18783=CARTESIAN_POINT('Origin',(46.5887585805977,107.052125922394,267.073593133701));
#18784=CARTESIAN_POINT('Origin',(46.4190297263865,206.75572924813,265.073593133701));
#18785=CARTESIAN_POINT('Origin',(46.4190297263865,206.75572924813,241.073593133701));
#18786=CARTESIAN_POINT('Origin',(-177.994184790505,208.37370585515,239.073593133701));
#18787=CARTESIAN_POINT('Origin',(-232.99410509728,208.28007760959,267.073593133701));
#18788=CARTESIAN_POINT('Origin',(76.9818224517878,206.807757335558,241.073593133701));
#18789=CARTESIAN_POINT('Origin',(76.9818224517878,206.807757335558,265.073593133701));
#18790=CARTESIAN_POINT('',(0.,0.,0.));
#18791=CARTESIAN_POINT('Origin',(37.0412526478464,187.739737607039,211.073593133701));
#18792=CARTESIAN_POINT('',(29.1412526478464,187.739737607039,211.573593133701));
#18793=CARTESIAN_POINT('Origin',(37.0412526478464,187.739737607039,211.573593133701));
#18794=CARTESIAN_POINT('',(29.6412526478464,187.739737607039,211.073593133701));
#18795=CARTESIAN_POINT('',(29.6412526478464,187.739737607039,211.073593133701));
#18796=CARTESIAN_POINT('Origin',(37.0412526478464,187.739737607039,211.073593133701));
#18797=CARTESIAN_POINT('Origin',(37.0412526479213,187.739737607024,242.073593133701));
#18798=CARTESIAN_POINT('',(50.0412526479213,187.739737607024,241.573593133701));
#18799=CARTESIAN_POINT('Origin',(37.0412526479213,187.739737607024,241.573593133701));
#18800=CARTESIAN_POINT('',(49.5412526479213,187.739737607024,242.073593133701));
#18801=CARTESIAN_POINT('',(49.5412526479213,187.739737607024,242.073593133701));
#18802=CARTESIAN_POINT('Origin',(37.0412526479213,187.739737607024,242.073593133701));
#18803=CARTESIAN_POINT('Origin',(37.0412526479213,187.739737607024,239.573593133701));
#18804=CARTESIAN_POINT('',(50.0412526479213,187.739737607024,239.573593133701));
#18805=CARTESIAN_POINT('',(24.0412526479213,187.739737607024,239.573593133701));
#18806=CARTESIAN_POINT('Origin',(37.0412526479213,187.739737607024,239.573593133701));
#18807=CARTESIAN_POINT('Origin',(37.0412526479213,187.739737607024,239.573593133701));
#18808=CARTESIAN_POINT('',(24.5412526479213,187.739737607024,239.073593133701));
#18809=CARTESIAN_POINT('',(24.0412526479213,187.739737607024,239.573593133701));
#18810=CARTESIAN_POINT('Origin',(37.0412526479213,187.739737607024,239.073593133701));
#18811=CARTESIAN_POINT('Origin',(37.0412526478464,187.739737607039,188.729018848206));
#18812=CARTESIAN_POINT('',(29.1412526478464,187.739737607039,239.073593133701));
#18813=CARTESIAN_POINT('Origin',(37.0412526478464,187.739737607039,239.073593133701));
#18814=CARTESIAN_POINT('',(29.1412526478464,187.739737607039,188.729018848206));
#18815=CARTESIAN_POINT('Origin',(37.0412526479213,187.739737607024,242.073593133701));
#18816=CARTESIAN_POINT('',(50.0412526479213,187.739737607024,242.073593133701));
#18817=CARTESIAN_POINT('Origin',(37.0412526479213,187.739737607024,242.073593133701));
#18818=CARTESIAN_POINT('Origin',(37.0412526479213,187.739737607024,239.073593133701));
#18819=CARTESIAN_POINT('Origin',(-276.958747352154,52.7397376070391,211.073593133701));
#18820=CARTESIAN_POINT('Origin',(37.0412526478464,187.739737607039,295.073593133701));
#18821=CARTESIAN_POINT('',(29.1412526478464,187.739737607039,294.573593133701));
#18822=CARTESIAN_POINT('Origin',(37.0412526478464,187.739737607039,294.573593133701));
#18823=CARTESIAN_POINT('',(29.6412526478464,187.739737607039,295.073593133701));
#18824=CARTESIAN_POINT('',(29.6412526478464,187.739737607039,295.073593133701));
#18825=CARTESIAN_POINT('Origin',(37.0412526478464,187.739737607039,295.073593133701));
#18826=CARTESIAN_POINT('Origin',(37.0412526479213,187.739737607024,264.073593133701));
#18827=CARTESIAN_POINT('',(50.0412526479213,187.739737607024,264.573593133701));
#18828=CARTESIAN_POINT('Origin',(37.0412526479213,187.739737607024,264.573593133701));
#18829=CARTESIAN_POINT('',(49.5412526479213,187.739737607024,264.073593133701));
#18830=CARTESIAN_POINT('',(49.5412526479213,187.739737607024,264.073593133701));
#18831=CARTESIAN_POINT('Origin',(37.0412526479213,187.739737607024,264.073593133701));
#18832=CARTESIAN_POINT('Origin',(37.0412526479213,187.739737607024,266.573593133701));
#18833=CARTESIAN_POINT('',(50.0412526479213,187.739737607024,266.573593133701));
#18834=CARTESIAN_POINT('',(24.0412526479213,187.739737607024,266.573593133701));
#18835=CARTESIAN_POINT('Origin',(37.0412526479213,187.739737607024,266.573593133701));
#18836=CARTESIAN_POINT('',(24.5412526479213,187.739737607024,267.073593133701));
#18837=CARTESIAN_POINT('',(24.0412526479213,187.739737607024,266.573593133701));
#18838=CARTESIAN_POINT('Origin',(37.0412526479213,187.739737607024,267.073593133701));
#18839=CARTESIAN_POINT('Origin',(37.0412526479213,187.739737607024,266.573593133701));
#18840=CARTESIAN_POINT('Origin',(37.0412526478464,187.739737607039,317.418167419196));
#18841=CARTESIAN_POINT('',(29.1412526478464,187.739737607039,267.073593133701));
#18842=CARTESIAN_POINT('Origin',(37.0412526478464,187.739737607039,267.073593133701));
#18843=CARTESIAN_POINT('',(29.1412526478464,187.739737607039,317.418167419196));
#18844=CARTESIAN_POINT('Origin',(37.0412526479213,187.739737607024,264.073593133701));
#18845=CARTESIAN_POINT('',(50.0412526479213,187.739737607024,264.073593133701));
#18846=CARTESIAN_POINT('Origin',(37.0412526479213,187.739737607024,264.073593133701));
#18847=CARTESIAN_POINT('Origin',(37.0412526479213,187.739737607024,267.073593133701));
#18848=CARTESIAN_POINT('Origin',(-276.958747352154,52.7397376070391,295.073593133701));
#18849=CARTESIAN_POINT('',(0.,0.,0.));
#18850=CARTESIAN_POINT('',(0.,0.,0.));
#18851=CARTESIAN_POINT('',(0.,0.,0.));
#18852=CARTESIAN_POINT('',(0.,0.,0.));
#18853=CARTESIAN_POINT('Origin',(-231.689233855248,191.349200530894,253.073593133704));
#18854=CARTESIAN_POINT('',(-223.099169485805,193.780362046156,262.048572120617));
#18855=CARTESIAN_POINT('',(-240.478663411414,192.913067616571,244.098614146791));
#18856=CARTESIAN_POINT('Origin',(-231.78891644861,193.346714831364,253.073593133704));
#18857=CARTESIAN_POINT('Origin',(-231.78891644861,193.346714831364,253.073593133704));
#18858=CARTESIAN_POINT('',(-238.988621304004,190.984936870468,245.534610784697));
#18859=CARTESIAN_POINT('',(-238.988621304004,190.984936870468,245.534610784697));
#18860=CARTESIAN_POINT('Origin',(-231.689233855248,191.349200530894,253.073593133704));
#18861=CARTESIAN_POINT('Origin',(-237.419514171664,306.176839858541,253.073593133704));
#18862=CARTESIAN_POINT('',(-250.440271285438,306.057676646063,218.820732405352));
#18863=CARTESIAN_POINT('',(-271.236343977855,305.019883596359,239.006032654733));
#18864=CARTESIAN_POINT('Origin',(-237.44592788123,306.706137510275,253.073593133704));
#18865=CARTESIAN_POINT('',(-251.347266456762,305.48179879318,218.618067764708));
#18866=CARTESIAN_POINT('Ctrl Pts',(-251.347266456762,305.48179879318,218.618067764708));
#18867=CARTESIAN_POINT('Ctrl Pts',(-250.891701988272,305.772942264292,218.717244054283));
#18868=CARTESIAN_POINT('Ctrl Pts',(-250.440271285437,306.057676646063,218.820732405352));
#18869=CARTESIAN_POINT('',(-271.383269500837,304.481935741607,238.065621311184));
#18870=CARTESIAN_POINT('Origin',(-237.419514171664,306.176839858541,253.073593133704));
#18871=CARTESIAN_POINT('Ctrl Pts',(-271.236343977855,305.019883596359,239.006032654733));
#18872=CARTESIAN_POINT('Ctrl Pts',(-271.312182393571,304.75389251631,238.537983013705));
#18873=CARTESIAN_POINT('Ctrl Pts',(-271.383269500837,304.481935741607,238.065621311184));
#18874=CARTESIAN_POINT('Origin',(-239.027345521937,338.395766018202,253.073593133704));
#18875=CARTESIAN_POINT('',(-264.591821718871,305.351467310312,259.227189433814));
#18876=CARTESIAN_POINT('',(-244.431608765165,306.35752884863,280.049140683453));
#18877=CARTESIAN_POINT('Origin',(-237.44592788123,306.706137510275,253.073593133704));
#18878=CARTESIAN_POINT('',(-243.894079636939,308.886976989217,282.887702827629));
#18879=CARTESIAN_POINT('Origin',(-221.806532920431,316.111846600949,269.669787882023));
#18880=CARTESIAN_POINT('',(-232.174356018737,309.471830095633,283.069881793484));
#18881=CARTESIAN_POINT('Origin',(-237.570506863568,309.202544258603,253.073593133704));
#18882=CARTESIAN_POINT('',(-231.299979576836,307.012840729122,280.253267222905));
#18883=CARTESIAN_POINT('Origin',(-254.450855472222,314.482786558815,269.162343413428));
#18884=CARTESIAN_POINT('',(-210.503906884418,308.050633778826,260.067966973523));
#18885=CARTESIAN_POINT('Origin',(-237.44592788123,306.706137510275,253.073593133704));
#18886=CARTESIAN_POINT('',(-207.793451628875,310.688518145128,259.405034938035));
#18887=CARTESIAN_POINT('Origin',(-221.299719129075,316.137138291257,236.984842853979));
#18888=CARTESIAN_POINT('',(-207.611499084105,310.697598181014,247.670727338388));
#18889=CARTESIAN_POINT('Origin',(-237.570506863568,309.202544258603,253.073593133704));
#18890=CARTESIAN_POINT('',(-210.300034043588,308.060807710239,246.919996833593));
#18891=CARTESIAN_POINT('Origin',(-221.806532920431,316.111846600949,269.669787882023));
#18892=CARTESIAN_POINT('',(-230.460246997295,307.054746171921,226.098045583955));
#18893=CARTESIAN_POINT('Origin',(-237.44592788123,306.706137510275,253.073593133704));
#18894=CARTESIAN_POINT('',(-231.246934090196,309.518111527989,223.259483439779));
#18895=CARTESIAN_POINT('Origin',(-253.944041680866,314.508078249123,236.477398385385));
#18896=CARTESIAN_POINT('',(-242.966657708398,308.933258421573,223.077304473924));
#18897=CARTESIAN_POINT('Origin',(-237.570506863568,309.202544258603,253.073593133704));
#18898=CARTESIAN_POINT('',(-243.591876185624,306.399434291429,225.893919044503));
#18899=CARTESIAN_POINT('Origin',(-221.299719129075,316.137138291257,236.984842853979));
#18900=CARTESIAN_POINT('',(-264.387948878041,305.361641241725,246.079219293884));
#18901=CARTESIAN_POINT('Origin',(-237.44592788123,306.706137510275,253.073593133704));
#18902=CARTESIAN_POINT('',(-267.347562098261,307.716570372078,246.742151329373));
#18903=CARTESIAN_POINT('Origin',(-254.450855472222,314.482786558815,269.162343413428));
#18904=CARTESIAN_POINT('',(-267.52951464303,307.707490336192,258.47645892902));
#18905=CARTESIAN_POINT('Origin',(-237.570506863568,309.202544258603,253.073593133704));
#18906=CARTESIAN_POINT('Origin',(-253.944041680866,314.508078249123,236.477398385385));
#18907=CARTESIAN_POINT('Origin',(-239.086294923286,339.57703817644,253.073593133704));
#18908=CARTESIAN_POINT('',(-252.408833339929,305.42882308236,287.079612836479));
#18909=CARTESIAN_POINT('',(-271.832216499046,304.459531796337,267.018677063088));
#18910=CARTESIAN_POINT('Origin',(-237.419514171664,306.176839858541,253.073593133704));
#18911=CARTESIAN_POINT('',(-272.435152125237,304.96005909095,266.840164323315));
#18912=CARTESIAN_POINT('Origin',(-254.384625574476,315.07819861504,236.052794955191));
#18913=CARTESIAN_POINT('',(-271.991461983488,304.982200701635,238.226128675688));
#18914=CARTESIAN_POINT('Origin',(-237.44592788123,306.706137510275,253.073593133704));
#18915=CARTESIAN_POINT('Origin',(-254.904405884816,315.052259852398,269.573964189148));
#18916=CARTESIAN_POINT('',(-251.19538929107,306.019993751338,218.040828426306));
#18917=CARTESIAN_POINT('Origin',(-220.905118117829,316.748937155912,236.573222078259));
#18918=CARTESIAN_POINT('',(-222.616916590929,307.446154391283,218.485070694454));
#18919=CARTESIAN_POINT('Origin',(-237.44592788123,306.706137510275,253.073593133704));
#18920=CARTESIAN_POINT('',(-222.4301950034,306.924856634723,219.067573430929));
#18921=CARTESIAN_POINT('Origin',(-254.384625574476,315.07819861504,236.052794955191));
#18922=CARTESIAN_POINT('',(-203.006811844283,307.894147920746,239.128509204319));
#18923=CARTESIAN_POINT('Origin',(-237.419514171664,306.176839858541,253.073593133704));
#18924=CARTESIAN_POINT('',(-202.456703637222,308.452215929601,239.307021944093));
#18925=CARTESIAN_POINT('Origin',(-221.42489842817,316.722998393271,270.094391312217));
#18926=CARTESIAN_POINT('',(-202.900393778972,308.430074318916,267.92105759172));
#18927=CARTESIAN_POINT('Origin',(-237.44592788123,306.706137510275,253.073593133704));
#18928=CARTESIAN_POINT('',(-203.455758842492,307.871743975476,268.081564956224));
#18929=CARTESIAN_POINT('Origin',(-220.905118117829,316.748937155912,236.573222078259));
#18930=CARTESIAN_POINT('',(-223.491761886567,306.871880923903,287.529118502699));
#18931=CARTESIAN_POINT('Origin',(-237.419514171664,306.176839858541,253.073593133704));
#18932=CARTESIAN_POINT('',(-223.696466471389,307.392281269213,288.106357841101));
#18933=CARTESIAN_POINT('Origin',(-254.904405884816,315.052259852398,269.573964189148));
#18934=CARTESIAN_POINT('',(-252.27493917153,305.966120629268,287.662115572953));
#18935=CARTESIAN_POINT('Origin',(-237.44592788123,306.706137510275,253.073593133704));
#18936=CARTESIAN_POINT('Origin',(-221.42489842817,316.722998393271,270.094391312217));
#18937=CARTESIAN_POINT('',(-227.983616560511,291.658562769169,262.048572120617));
#18938=CARTESIAN_POINT('Origin',(-236.673363523316,291.224915554376,253.073593133704));
#18939=CARTESIAN_POINT('Origin',(-231.689233855248,191.349200530894,253.073593133704));
#18940=CARTESIAN_POINT('',(-222.999486892444,191.782847745686,262.048572120617));
#18941=CARTESIAN_POINT('Origin',(-237.670189456929,311.200058559073,253.073593133704));
#18942=CARTESIAN_POINT('',(-228.761753229824,309.64213030126,286.594499765937));
#18943=CARTESIAN_POINT('Ctrl Pts',(-223.69646647139,307.392281269213,288.106357841101));
#18944=CARTESIAN_POINT('Ctrl Pts',(-226.31000387672,308.600428762359,287.396575304205));
#18945=CARTESIAN_POINT('Ctrl Pts',(-228.761753229824,309.64213030126,286.594499765937));
#18946=CARTESIAN_POINT('',(-247.414317038773,308.711305459166,286.304552247041));
#18947=CARTESIAN_POINT('Origin',(-237.570506863568,309.202544258603,253.073593133704));
#18948=CARTESIAN_POINT('Ctrl Pts',(-247.414317038773,308.711305459166,286.304552247041));
#18949=CARTESIAN_POINT('Ctrl Pts',(-249.773889204424,307.429503007661,287.031837490994));
#18950=CARTESIAN_POINT('Ctrl Pts',(-252.274939171527,305.96612062927,287.662115572952));
#18951=CARTESIAN_POINT('Origin',(-237.670189456929,311.200058559073,253.073593133704));
#18952=CARTESIAN_POINT('',(-271.049752044865,307.531818806141,261.893308348431));
#18953=CARTESIAN_POINT('Ctrl Pts',(-272.435152125237,304.96005909095,266.840164323315));
#18954=CARTESIAN_POINT('Ctrl Pts',(-271.792884971683,306.33068203763,264.290090789975));
#18955=CARTESIAN_POINT('Ctrl Pts',(-271.049752044865,307.531818806141,261.893308348431));
#18956=CARTESIAN_POINT('',(-270.760164887174,307.546270166452,243.217533356919));
#18957=CARTESIAN_POINT('Origin',(-237.570506863568,309.202544258603,253.073593133704));
#18958=CARTESIAN_POINT('Ctrl Pts',(-270.760164887174,307.546270166452,243.217533356919));
#18959=CARTESIAN_POINT('Ctrl Pts',(-271.428600472778,306.348861043188,240.797007088707));
#18960=CARTESIAN_POINT('Ctrl Pts',(-271.991461983488,304.982200701635,238.226128675688));
#18961=CARTESIAN_POINT('Origin',(-237.670189456929,311.200058559073,253.073593133704));
#18962=CARTESIAN_POINT('',(-204.09126168227,310.873269711066,244.253877918976));
#18963=CARTESIAN_POINT('Ctrl Pts',(-202.456703637222,308.452215929601,239.307021944093));
#18964=CARTESIAN_POINT('Ctrl Pts',(-203.232237251341,309.75208591228,241.857095477433));
#18965=CARTESIAN_POINT('Ctrl Pts',(-204.09126168227,310.873269711065,244.253877918976));
#18966=CARTESIAN_POINT('',(-204.380848839961,310.858818350754,262.929652910489));
#18967=CARTESIAN_POINT('Origin',(-237.570506863568,309.202544258603,253.073593133704));
#18968=CARTESIAN_POINT('Ctrl Pts',(-204.380848839961,310.858818350754,262.929652910489));
#18969=CARTESIAN_POINT('Ctrl Pts',(-203.596521750247,309.733906906721,265.350179178701));
#18970=CARTESIAN_POINT('Ctrl Pts',(-202.900393778972,308.430074318916,267.92105759172));
#18971=CARTESIAN_POINT('Origin',(-231.689233855248,191.349200530894,253.073593133704));
#18972=CARTESIAN_POINT('Origin',(-237.670189456929,311.200058559073,253.073593133704));
#18973=CARTESIAN_POINT('',(-246.379260497312,308.762958215947,219.55268650147));
#18974=CARTESIAN_POINT('Ctrl Pts',(-251.195389291067,306.019993751341,218.040828426307));
#18975=CARTESIAN_POINT('Ctrl Pts',(-248.715118346303,307.482339187552,218.750610963203));
#18976=CARTESIAN_POINT('Ctrl Pts',(-246.379260497312,308.762958215947,219.55268650147));
#18977=CARTESIAN_POINT('',(-227.726696688362,309.69378305804,219.842634020367));
#18978=CARTESIAN_POINT('Origin',(-237.570506863568,309.202544258603,253.073593133704));
#18979=CARTESIAN_POINT('Ctrl Pts',(-227.726696688362,309.69378305804,219.842634020367));
#18980=CARTESIAN_POINT('Ctrl Pts',(-225.251233018599,308.65326494225,219.115348776413));
#18981=CARTESIAN_POINT('Ctrl Pts',(-222.61691659093,307.446154391284,218.485070694455));
#18982=CARTESIAN_POINT('Origin',(-254.358103779067,305.86216380131,289.684098458565));
#18983=CARTESIAN_POINT('',(-203.23563831279,308.413344503999,240.063079615825));
#18984=CARTESIAN_POINT('',(-254.358103779067,305.86216380131,289.684098458565));
#18985=CARTESIAN_POINT('',(-223.395851266497,307.407282965681,219.241128366186));
#18986=CARTESIAN_POINT('Origin',(-237.44592788123,306.706137510275,253.073593133704));
#18987=CARTESIAN_POINT('',(-274.518316732773,304.856102262992,268.862147208927));
#18988=CARTESIAN_POINT('Origin',(-274.518316732773,304.856102262992,268.862147208927));
#18989=CARTESIAN_POINT('',(-276.380506741304,307.265796453966,267.067500884441));
#18990=CARTESIAN_POINT('Ctrl Pts',(-223.395851266497,307.407282965681,219.241128366186));
#18991=CARTESIAN_POINT('Ctrl Pts',(-222.915330871771,307.169056036833,219.152126865893));
#18992=CARTESIAN_POINT('Ctrl Pts',(-222.4301950034,306.924856634723,219.067573430929));
#18993=CARTESIAN_POINT('Origin',(-251.454394814525,310.512180961828,292.914741420956));
#18994=CARTESIAN_POINT('',(-252.745071735212,308.445283106991,291.47874478305));
#18995=CARTESIAN_POINT('Ctrl Pts',(-203.006811844283,307.894147920746,239.128509204319));
#18996=CARTESIAN_POINT('Ctrl Pts',(-203.11922611311,308.156947367739,239.598018442737));
#18997=CARTESIAN_POINT('Ctrl Pts',(-203.23563831279,308.413344503999,240.063079615825));
#18998=CARTESIAN_POINT('Origin',(-251.454394814525,310.512180961828,292.914741420956));
#18999=CARTESIAN_POINT('',(-252.745071735212,308.445283106991,291.47874478305));
#19000=CARTESIAN_POINT('',(-251.496004495962,306.00499205487,286.906057901221));
#19001=CARTESIAN_POINT('',(-254.358103779067,305.86216380131,289.684098458565));
#19002=CARTESIAN_POINT('Ctrl Pts',(-251.496004495962,306.00499205487,286.906057901221));
#19003=CARTESIAN_POINT('Ctrl Pts',(-251.950419952519,305.720108723982,286.995059401515));
#19004=CARTESIAN_POINT('Ctrl Pts',(-252.408833339929,305.42882308236,287.079612836479));
#19005=CARTESIAN_POINT('Origin',(-274.518316732773,304.856102262992,268.862147208927));
#19006=CARTESIAN_POINT('',(-276.380506741304,307.265796453966,267.067500884441));
#19007=CARTESIAN_POINT('',(-271.656217449669,304.998930516552,266.084106651583));
#19008=CARTESIAN_POINT('Ctrl Pts',(-271.832216499046,304.459531796337,267.018677063088));
#19009=CARTESIAN_POINT('Ctrl Pts',(-271.746524711181,304.732217393075,266.549167824671));
#19010=CARTESIAN_POINT('Ctrl Pts',(-271.656217449669,304.998930516552,266.084106651583));
#19011=CARTESIAN_POINT('',(-274.518316732773,304.856102262992,268.862147208927));
#19012=CARTESIAN_POINT('Origin',(-254.358103779067,305.86216380131,289.684098458565));
#19013=CARTESIAN_POINT('Origin',(-237.44592788123,306.706137510275,253.073593133704));
#19014=CARTESIAN_POINT('Origin',(-274.010931848145,304.88142245275,236.14037178569));
#19015=CARTESIAN_POINT('',(-253.214859155728,305.919215502453,215.955071536309));
#19016=CARTESIAN_POINT('',(-274.010931848145,304.88142245275,236.14037178569));
#19017=CARTESIAN_POINT('Origin',(-253.214859155728,305.919215502453,215.955071536309));
#19018=CARTESIAN_POINT('',(-251.547022289343,308.505069750677,214.215298233275));
#19019=CARTESIAN_POINT('Origin',(-277.461821182389,309.214324067189,239.272234761095));
#19020=CARTESIAN_POINT('',(-275.927926679205,307.288381701182,237.880145088724));
#19021=CARTESIAN_POINT('Origin',(-277.461821182389,309.214324067189,239.272234761095));
#19022=CARTESIAN_POINT('',(-275.927926679205,307.288381701182,237.880145088724));
#19023=CARTESIAN_POINT('',(-224.451584477021,307.354598374488,287.326453862056));
#19024=CARTESIAN_POINT('Ctrl Pts',(-223.491761886567,306.871880923903,287.529118502699));
#19025=CARTESIAN_POINT('Ctrl Pts',(-223.974048836019,307.116222496522,287.429942213125));
#19026=CARTESIAN_POINT('Ctrl Pts',(-224.451584477021,307.354598374488,287.326453862056));
#19027=CARTESIAN_POINT('',(-274.010931848145,304.88142245275,236.14037178569));
#19028=CARTESIAN_POINT('Origin',(-253.214859155728,305.919215502453,215.955071536309));
#19029=CARTESIAN_POINT('',(-251.547022289343,308.505069750677,214.215298233275));
#19030=CARTESIAN_POINT('',(-203.655511784604,308.392391424192,267.141153612674));
#19031=CARTESIAN_POINT('',(-253.214859155728,305.919215502453,215.955071536309));
#19032=CARTESIAN_POINT('Ctrl Pts',(-203.655511784604,308.392391424192,267.141153612674));
#19033=CARTESIAN_POINT('Ctrl Pts',(-203.55356843072,308.135272244505,267.609203253702));
#19034=CARTESIAN_POINT('Ctrl Pts',(-203.455758842491,307.871743975476,268.081564956224));
#19035=CARTESIAN_POINT('Origin',(-274.010931848145,304.88142245275,236.14037178569));
#19036=CARTESIAN_POINT('Origin',(-237.44592788123,306.706137510275,253.073593133704));
#19037=CARTESIAN_POINT('Origin',(-240.071393924063,309.077741693818,304.568423058936));
#19038=CARTESIAN_POINT('Origin',(-240.071393924063,309.077741693818,304.568423058936));
#19039=CARTESIAN_POINT('Origin',(-240.071393924063,309.077741693818,304.568423058936));
#19040=CARTESIAN_POINT('Origin',(-240.071393924063,309.077741693818,304.568423058936));
#19041=CARTESIAN_POINT('Origin',(-237.419514171664,306.176839858541,253.073593133704));
#19042=CARTESIAN_POINT('Origin',(-237.419514171664,306.176839858541,253.073593133704));
#19043=CARTESIAN_POINT('Origin',(-237.419514171664,306.176839858541,253.073593133704));
#19044=CARTESIAN_POINT('',(0.,0.,0.));
#19045=CARTESIAN_POINT('Origin',(-235.27780721626,263.259715347801,253.073593133701));
#19046=CARTESIAN_POINT('',(-235.27780721626,263.259715347801,239.573593133701));
#19047=CARTESIAN_POINT('Origin',(-235.27780721626,263.259715347801,253.073593133701));
#19048=CARTESIAN_POINT('',(-235.327648512941,264.258472498036,238.573593133701));
#19049=CARTESIAN_POINT('',(-235.27780721626,263.259715347801,239.573593133701));
#19050=CARTESIAN_POINT('Origin',(-235.327648512941,264.258472498036,253.073593133701));
#19051=CARTESIAN_POINT('Origin',(-232.939627118478,176.278148255512,236.573593133701));
#19052=CARTESIAN_POINT('',(-232.192007668268,161.29679100199,234.573593133701));
#19053=CARTESIAN_POINT('Origin',(-232.939627118478,176.278148255512,234.573593133701));
#19054=CARTESIAN_POINT('',(-232.29169026163,163.29430530246,236.573593133701));
#19055=CARTESIAN_POINT('Origin',(-232.192007668268,161.29679100199,236.573593133701));
#19056=CARTESIAN_POINT('',(-219.955784165426,176.926085112361,236.573593133701));
#19057=CARTESIAN_POINT('Origin',(-232.939627118478,176.278148255512,236.573593133701));
#19058=CARTESIAN_POINT('Origin',(-232.939627118478,176.278148255512,236.573593133701));
#19059=CARTESIAN_POINT('Origin',(-232.939627118478,176.278148255512,269.573593133701));
#19060=CARTESIAN_POINT('',(-233.687246568689,191.259505509035,271.573593133701));
#19061=CARTESIAN_POINT('Origin',(-232.939627118478,176.278148255512,271.573593133701));
#19062=CARTESIAN_POINT('',(-233.587563975327,189.261991208565,269.573593133701));
#19063=CARTESIAN_POINT('Origin',(-233.687246568688,191.259505509035,269.573593133701));
#19064=CARTESIAN_POINT('',(-219.955784165426,176.926085112361,269.573593133701));
#19065=CARTESIAN_POINT('Origin',(-232.939627118478,176.278148255512,269.573593133701));
#19066=CARTESIAN_POINT('Origin',(-232.939627118478,176.278148255512,269.573593133701));
#19067=CARTESIAN_POINT('Origin',(-232.939627118478,176.278148255512,276.575593133701));
#19068=CARTESIAN_POINT('',(-219.955784165426,176.926085112361,276.575593133701));
#19069=CARTESIAN_POINT('Origin',(-234.829235546134,254.270900995688,253.073593133701));
#19070=CARTESIAN_POINT('',(-234.829235546134,254.270900995688,240.573593133701));
#19071=CARTESIAN_POINT('Origin',(-234.829235546134,254.270900995688,253.073593133701));
#19072=CARTESIAN_POINT('',(-235.078442029538,259.264686746862,240.573593133701));
#19073=CARTESIAN_POINT('',(-234.829235546134,254.270900995688,240.573593133701));
#19074=CARTESIAN_POINT('Origin',(-235.078442029538,259.264686746862,253.073593133701));
#19075=CARTESIAN_POINT('Origin',(-234.829235546134,254.270900995688,253.073593133701));
#19076=CARTESIAN_POINT('',(-225.938313363545,259.720809503464,268.573593133701));
#19077=CARTESIAN_POINT('',(-244.218570695531,258.80856399026,268.573593133701));
#19078=CARTESIAN_POINT('Ctrl Pts',(-244.218570695531,258.80856399026,268.573593133701));
#19079=CARTESIAN_POINT('Ctrl Pts',(-243.882569447187,258.825331567743,268.772221695988));
#19080=CARTESIAN_POINT('Ctrl Pts',(-243.537504054999,258.822928410752,268.960846032026));
#19081=CARTESIAN_POINT('Ctrl Pts',(-242.350109030347,258.767377256699,269.558780483369));
#19082=CARTESIAN_POINT('Ctrl Pts',(-241.471668538286,258.64932649441,269.917592682587));
#19083=CARTESIAN_POINT('Ctrl Pts',(-238.761208602761,258.222554255849,270.783055750245));
#19084=CARTESIAN_POINT('Ctrl Pts',(-236.856253783888,257.832610843749,271.073593133701));
#19085=CARTESIAN_POINT('Ctrl Pts',(-233.166887375258,258.01672247258,271.073593133701));
#19086=CARTESIAN_POINT('Ctrl Pts',(-231.310219222211,258.594383355839,270.783055750245));
#19087=CARTESIAN_POINT('Ctrl Pts',(-228.655714581594,259.288885133116,269.917592682587));
#19088=CARTESIAN_POINT('Ctrl Pts',(-227.793391434726,259.493805778597,269.558780483369));
#19089=CARTESIAN_POINT('Ctrl Pts',(-226.617426357145,259.667296445764,268.960846032026));
#19090=CARTESIAN_POINT('Ctrl Pts',(-226.274314611889,259.704041925981,268.772221695988));
#19091=CARTESIAN_POINT('Ctrl Pts',(-225.938313363545,259.720809503464,268.573593133701));
#19092=CARTESIAN_POINT('',(-244.218570695531,258.80856399026,237.573593133701));
#19093=CARTESIAN_POINT('Origin',(-235.078442029538,259.264686746862,253.073593133701));
#19094=CARTESIAN_POINT('',(-235.011570579573,257.924666658164,235.073593133701));
#19095=CARTESIAN_POINT('Ctrl Pts',(-244.218570695531,258.80856399026,237.573593133701));
#19096=CARTESIAN_POINT('Ctrl Pts',(-243.882569447187,258.825331567743,237.374964571413));
#19097=CARTESIAN_POINT('Ctrl Pts',(-243.537504054999,258.822928410752,237.186340235375));
#19098=CARTESIAN_POINT('Ctrl Pts',(-242.350109030347,258.767377256699,236.588405784032));
#19099=CARTESIAN_POINT('Ctrl Pts',(-241.471668538286,258.64932649441,236.229593584814));
#19100=CARTESIAN_POINT('Ctrl Pts',(-238.761208602761,258.222554255849,235.364130517157));
#19101=CARTESIAN_POINT('Ctrl Pts',(-236.856253783888,257.832610843749,235.073593133701));
#19102=CARTESIAN_POINT('Ctrl Pts',(-235.011570579573,257.924666658164,235.073593133701));
#19103=CARTESIAN_POINT('',(-234.829235546134,254.270900995688,235.073593133701));
#19104=CARTESIAN_POINT('',(-234.829235546134,254.270900995688,235.073593133701));
#19105=CARTESIAN_POINT('Origin',(-234.829235546134,254.270900995688,253.073593133701));
#19106=CARTESIAN_POINT('',(-225.938313363544,259.720809503464,237.573593133701));
#19107=CARTESIAN_POINT('Ctrl Pts',(-235.011570579573,257.924666658164,235.073593133701));
#19108=CARTESIAN_POINT('Ctrl Pts',(-233.166887375258,258.01672247258,235.073593133701));
#19109=CARTESIAN_POINT('Ctrl Pts',(-231.310219222211,258.594383355839,235.364130517156));
#19110=CARTESIAN_POINT('Ctrl Pts',(-228.655714581594,259.288885133116,236.229593584814));
#19111=CARTESIAN_POINT('Ctrl Pts',(-227.793391434726,259.493805778597,236.588405784032));
#19112=CARTESIAN_POINT('Ctrl Pts',(-226.617426357145,259.667296445764,237.186340235375));
#19113=CARTESIAN_POINT('Ctrl Pts',(-226.274314611889,259.704041925981,237.374964571413));
#19114=CARTESIAN_POINT('Ctrl Pts',(-225.938313363545,259.720809503464,237.573593133701));
#19115=CARTESIAN_POINT('Origin',(-235.078442029538,259.264686746862,253.073593133701));
#19116=CARTESIAN_POINT('Origin',(-231.779757303713,193.163177041049,253.073593133701));
#19117=CARTESIAN_POINT('',(-233.682885722479,231.299486540287,239.573593133701));
#19118=CARTESIAN_POINT('Origin',(-233.682885722479,231.299486540287,253.073593133701));
#19119=CARTESIAN_POINT('',(-233.932092205882,236.293272291461,239.573593133701));
#19120=CARTESIAN_POINT('',(-231.779757303713,193.163177041049,239.573593133701));
#19121=CARTESIAN_POINT('Origin',(-233.932092205882,236.293272291461,253.073593133701));
#19122=CARTESIAN_POINT('Origin',(-231.779757303713,193.163177041049,253.073593133701));
#19123=CARTESIAN_POINT('',(-235.078442029538,259.264686746862,239.573593133701));
#19124=CARTESIAN_POINT('Origin',(-235.078442029538,259.264686746862,253.073593133701));
#19125=CARTESIAN_POINT('',(-231.779757303713,193.163177041049,239.573593133701));
#19126=CARTESIAN_POINT('Origin',(-232.939627118478,176.278148255512,276.573593133701));
#19127=CARTESIAN_POINT('',(-224.9495699166,176.676878628958,276.573593133701));
#19128=CARTESIAN_POINT('Origin',(-232.939627118478,176.278148255512,276.573593133701));
#19129=CARTESIAN_POINT('',(-224.9495699166,176.676878628958,229.573593133701));
#19130=CARTESIAN_POINT('',(-224.9495699166,176.676878628958,276.573593133701));
#19131=CARTESIAN_POINT('Origin',(-232.939627118478,176.278148255512,229.573593133701));
#19132=CARTESIAN_POINT('Origin',(-256.262104047518,132.050757761675,276.573593133701));
#19133=CARTESIAN_POINT('',(-248.272046845639,132.44948813512,276.573593133701));
#19134=CARTESIAN_POINT('Origin',(-256.262104047518,132.050757761675,276.573593133701));
#19135=CARTESIAN_POINT('',(-248.272046845639,132.44948813512,271.573593133701));
#19136=CARTESIAN_POINT('',(-248.272046845639,132.44948813512,276.573593133701));
#19137=CARTESIAN_POINT('Origin',(-256.262104047518,132.050757761675,271.573593133701));
#19138=CARTESIAN_POINT('Origin',(-256.262104047518,132.050757761675,276.573593133701));
#19139=CARTESIAN_POINT('',(-245.281648262624,121.831678020525,234.573593133701));
#19140=CARTESIAN_POINT('',(-270.702967511588,136.108030541768,234.573593133701));
#19141=CARTESIAN_POINT('Origin',(-256.262104047518,132.050757761675,234.573593133701));
#19142=CARTESIAN_POINT('',(-270.702967511588,136.108030541768,229.573593133701));
#19143=CARTESIAN_POINT('',(-270.702967511588,136.108030541768,276.573593133701));
#19144=CARTESIAN_POINT('',(-245.281648262624,121.831678020525,229.573593133701));
#19145=CARTESIAN_POINT('Origin',(-256.262104047518,132.050757761675,229.573593133701));
#19146=CARTESIAN_POINT('',(-245.281648262624,121.831678020525,276.573593133701));
#19147=CARTESIAN_POINT('Origin',(-256.262104047518,132.050757761675,276.573593133701));
#19148=CARTESIAN_POINT('',(-248.272046845639,132.44948813512,234.573593133701));
#19149=CARTESIAN_POINT('Origin',(-256.262104047518,132.050757761675,234.573593133701));
#19150=CARTESIAN_POINT('',(-248.272046845639,132.44948813512,229.573593133701));
#19151=CARTESIAN_POINT('',(-248.272046845639,132.44948813512,276.573593133701));
#19152=CARTESIAN_POINT('Origin',(-256.262104047518,132.050757761675,229.573593133701));
#19153=CARTESIAN_POINT('Origin',(-256.262104047518,132.050757761675,276.573593133701));
#19154=CARTESIAN_POINT('',(-270.702967511588,136.108030541768,276.573593133701));
#19155=CARTESIAN_POINT('',(-245.281648262624,121.831678020525,276.573593133701));
#19156=CARTESIAN_POINT('Origin',(-256.262104047518,132.050757761675,276.573593133701));
#19157=CARTESIAN_POINT('',(-270.702967511588,136.108030541768,271.573593133701));
#19158=CARTESIAN_POINT('',(-270.702967511588,136.108030541768,276.573593133701));
#19159=CARTESIAN_POINT('',(-245.281648262624,121.831678020525,271.573593133701));
#19160=CARTESIAN_POINT('Origin',(-256.262104047518,132.050757761675,271.573593133701));
#19161=CARTESIAN_POINT('',(-245.281648262624,121.831678020525,276.573593133701));
#19162=CARTESIAN_POINT('Origin',(-277.373940792763,254.150267790348,268.573593133701));
#19163=CARTESIAN_POINT('',(-205.115727522493,260.759925647282,268.573593133701));
#19164=CARTESIAN_POINT('',(-277.523464682805,257.146539241052,268.573593133701));
#19165=CARTESIAN_POINT('',(-204.966203632451,257.763654196578,271.573593133701));
#19166=CARTESIAN_POINT('Origin',(-204.966203632451,257.763654196578,268.573593133701));
#19167=CARTESIAN_POINT('',(-264.89163264654,254.773176395737,271.573593133701));
#19168=CARTESIAN_POINT('',(-277.373940792763,254.150267790348,271.573593133701));
#19169=CARTESIAN_POINT('',(-265.041156536582,257.769447846442,268.573593133701));
#19170=CARTESIAN_POINT('Origin',(-264.89163264654,254.773176395737,268.573593133701));
#19171=CARTESIAN_POINT('',(-277.523464682805,257.146539241052,268.573593133701));
#19172=CARTESIAN_POINT('Origin',(-277.523464682805,257.146539241052,237.573593133701));
#19173=CARTESIAN_POINT('',(-265.041156536582,257.769447846442,237.573593133701));
#19174=CARTESIAN_POINT('',(-265.041156536582,257.769447846442,276.573593133701));
#19175=CARTESIAN_POINT('',(-277.523464682805,257.146539241052,237.573593133701));
#19176=CARTESIAN_POINT('Origin',(-277.373940792763,254.150267790348,237.573593133701));
#19177=CARTESIAN_POINT('',(-264.89163264654,254.773176395737,234.573593133701));
#19178=CARTESIAN_POINT('Origin',(-264.89163264654,254.773176395737,237.573593133701));
#19179=CARTESIAN_POINT('',(-204.966203632451,257.763654196578,234.573593133701));
#19180=CARTESIAN_POINT('',(-277.373940792763,254.150267790348,234.573593133701));
#19181=CARTESIAN_POINT('',(-205.115727522493,260.759925647282,237.573593133701));
#19182=CARTESIAN_POINT('Origin',(-204.966203632451,257.763654196578,237.573593133701));
#19183=CARTESIAN_POINT('',(-277.523464682805,257.146539241052,237.573593133701));
#19184=CARTESIAN_POINT('Origin',(-260.739538157925,171.570404093794,276.573593133701));
#19185=CARTESIAN_POINT('',(-261.622986471561,168.425987347309,234.573593133701));
#19186=CARTESIAN_POINT('',(-260.739538157925,171.570404093794,234.573593133701));
#19187=CARTESIAN_POINT('',(-261.622986471561,168.425987347309,229.573593133701));
#19188=CARTESIAN_POINT('',(-261.622986471561,168.425987347309,229.573593133701));
#19189=CARTESIAN_POINT('',(-260.739538157925,171.570404093794,229.573593133701));
#19190=CARTESIAN_POINT('Origin',(-245.281648262624,121.831678020525,276.573593133701));
#19191=CARTESIAN_POINT('',(-206.335336816992,163.679697768471,229.573593133701));
#19192=CARTESIAN_POINT('',(-245.281648262624,121.831678020525,229.573593133701));
#19193=CARTESIAN_POINT('',(-206.335336816992,163.679697768471,234.573593133701));
#19194=CARTESIAN_POINT('',(-206.335336816992,163.679697768471,276.573593133701));
#19195=CARTESIAN_POINT('',(-245.281648262624,121.831678020525,234.573593133701));
#19196=CARTESIAN_POINT('Origin',(-256.262104047518,132.050757761675,276.573593133701));
#19197=CARTESIAN_POINT('',(-206.335336816992,163.679697768471,276.573593133701));
#19198=CARTESIAN_POINT('',(-245.281648262624,121.831678020525,276.573593133701));
#19199=CARTESIAN_POINT('',(-201.000801525488,178.301963356951,276.573593133701));
#19200=CARTESIAN_POINT('Origin',(-220.975944530184,177.305137423337,276.573593133701));
#19201=CARTESIAN_POINT('',(-204.966203632451,257.763654196578,276.573593133701));
#19202=CARTESIAN_POINT('',(-200.579725765336,169.864132597105,276.573593133701));
#19203=CARTESIAN_POINT('',(-264.89163264654,254.773176395737,276.573593133701));
#19204=CARTESIAN_POINT('',(-264.89163264654,254.773176395737,276.573593133701));
#19205=CARTESIAN_POINT('',(-260.902328085625,174.832510321047,276.573593133701));
#19206=CARTESIAN_POINT('',(-265.290363019986,262.763233597616,276.573593133701));
#19207=CARTESIAN_POINT('',(-261.622986471561,168.425987347309,276.573593133701));
#19208=CARTESIAN_POINT('Origin',(-280.877471090321,173.835684387434,276.573593133701));
#19209=CARTESIAN_POINT('',(-260.739538157925,171.570404093794,276.573593133701));
#19210=CARTESIAN_POINT('Origin',(-256.262104047518,132.050757761675,229.573593133701));
#19211=CARTESIAN_POINT('',(-201.000801525488,178.301963356951,229.573593133701));
#19212=CARTESIAN_POINT('',(-204.966203632451,257.763654196578,229.573593133701));
#19213=CARTESIAN_POINT('',(-200.579725765336,169.864132597105,229.573593133701));
#19214=CARTESIAN_POINT('Origin',(-220.975944530184,177.305137423337,229.573593133701));
#19215=CARTESIAN_POINT('',(-260.902328085625,174.832510321047,229.573593133701));
#19216=CARTESIAN_POINT('Origin',(-280.877471090321,173.835684387434,229.573593133701));
#19217=CARTESIAN_POINT('',(-264.89163264654,254.773176395737,229.573593133701));
#19218=CARTESIAN_POINT('',(-265.290363019986,262.763233597616,229.573593133701));
#19219=CARTESIAN_POINT('',(-262.39258353924,254.897887240558,229.573593133701));
#19220=CARTESIAN_POINT('Origin',(-205.364934005896,265.753711398456,276.573593133701));
#19221=CARTESIAN_POINT('',(-205.364934005896,265.753711398456,268.573593133701));
#19222=CARTESIAN_POINT('',(-205.364934005896,265.753711398456,237.573593133701));
#19223=CARTESIAN_POINT('',(-205.364934005896,265.753711398456,276.573593133701));
#19224=CARTESIAN_POINT('',(-265.290363019986,262.763233597616,237.573593133701));
#19225=CARTESIAN_POINT('',(-205.364934005896,265.753711398456,237.573593133701));
#19226=CARTESIAN_POINT('',(-265.290363019986,262.763233597616,268.573593133701));
#19227=CARTESIAN_POINT('',(-265.290363019986,262.763233597616,276.573593133701));
#19228=CARTESIAN_POINT('',(-205.364934005896,265.753711398456,268.573593133701));
#19229=CARTESIAN_POINT('Origin',(-265.290363019986,262.763233597616,276.573593133701));
#19230=CARTESIAN_POINT('',(-263.645600229524,229.804247639867,271.573593133701));
#19231=CARTESIAN_POINT('',(-260.902328085625,174.832510321047,271.573593133701));
#19232=CARTESIAN_POINT('',(-265.290363019986,262.763233597616,271.573593133701));
#19233=CARTESIAN_POINT('',(-260.902328085625,174.832510321047,276.573593133701));
#19234=CARTESIAN_POINT('Origin',(-264.89163264654,254.773176395737,268.573593133701));
#19235=CARTESIAN_POINT('Origin',(-264.89163264654,254.773176395737,237.573593133701));
#19236=CARTESIAN_POINT('',(-260.902328085625,174.832510321047,234.573593133701));
#19237=CARTESIAN_POINT('',(-260.902328085625,174.832510321047,234.573593133701));
#19238=CARTESIAN_POINT('',(-263.645600229524,229.804247639867,234.573593133701));
#19239=CARTESIAN_POINT('',(-265.290363019986,262.763233597616,234.573593133701));
#19240=CARTESIAN_POINT('',(-263.645600229524,229.804247639867,276.573593133701));
#19241=CARTESIAN_POINT('',(-263.894806712927,234.798033391041,271.573593133701));
#19242=CARTESIAN_POINT('',(-265.290363019986,262.763233597616,271.573593133701));
#19243=CARTESIAN_POINT('',(-263.894806712927,234.798033391041,234.573593133701));
#19244=CARTESIAN_POINT('',(-263.894806712927,234.798033391041,276.573593133701));
#19245=CARTESIAN_POINT('',(-265.290363019986,262.763233597616,234.573593133701));
#19246=CARTESIAN_POINT('Origin',(-260.739538157925,171.570404093794,276.573593133701));
#19247=CARTESIAN_POINT('',(-261.622986471561,168.425987347309,271.573593133701));
#19248=CARTESIAN_POINT('',(-261.622986471561,168.425987347309,271.573593133701));
#19249=CARTESIAN_POINT('',(-260.739538157925,171.570404093794,271.573593133701));
#19250=CARTESIAN_POINT('Origin',(-245.281648262624,121.831678020525,276.573593133701));
#19251=CARTESIAN_POINT('',(-206.335336816992,163.679697768471,271.573593133701));
#19252=CARTESIAN_POINT('',(-245.281648262624,121.831678020525,271.573593133701));
#19253=CARTESIAN_POINT('',(-206.335336816992,163.679697768471,276.573593133701));
#19254=CARTESIAN_POINT('Origin',(-200.579725765336,169.864132597105,276.573593133701));
#19255=CARTESIAN_POINT('',(-201.000801525488,178.301963356951,234.573593133701));
#19256=CARTESIAN_POINT('',(-203.720171215434,232.794725440707,234.573593133701));
#19257=CARTESIAN_POINT('',(-198.088104690518,119.935167464172,234.573593133701));
#19258=CARTESIAN_POINT('',(-201.000801525488,178.301963356951,276.573593133701));
#19259=CARTESIAN_POINT('Origin',(-204.966203632451,257.763654196578,237.573593133701));
#19260=CARTESIAN_POINT('Origin',(-204.966203632451,257.763654196578,268.573593133701));
#19261=CARTESIAN_POINT('',(-201.000801525488,178.301963356951,271.573593133701));
#19262=CARTESIAN_POINT('',(-201.000801525488,178.301963356951,276.573593133701));
#19263=CARTESIAN_POINT('',(-203.720171215434,232.794725440707,271.573593133701));
#19264=CARTESIAN_POINT('',(-203.720171215434,232.794725440707,271.573593133701));
#19265=CARTESIAN_POINT('',(-203.720171215434,232.794725440707,234.573593133701));
#19266=CARTESIAN_POINT('',(-203.969377698837,237.788511191881,234.573593133701));
#19267=CARTESIAN_POINT('',(-203.969377698837,237.788511191881,234.573593133701));
#19268=CARTESIAN_POINT('',(-203.969377698837,237.788511191881,271.573593133701));
#19269=CARTESIAN_POINT('',(-203.969377698837,237.788511191881,271.573593133701));
#19270=CARTESIAN_POINT('',(-204.966203632451,257.763654196578,271.573593133701));
#19271=CARTESIAN_POINT('',(-205.115727522493,260.759925647282,237.573593133701));
#19272=CARTESIAN_POINT('Origin',(-204.966203632451,257.763654196578,237.573593133701));
#19273=CARTESIAN_POINT('Origin',(-262.39258353924,254.897887240558,268.573593133701));
#19274=CARTESIAN_POINT('Origin',(-276.127908375746,229.181339034477,234.573593133701));
#19275=CARTESIAN_POINT('',(-276.127908375746,229.181339034477,234.573593133701));
#19276=CARTESIAN_POINT('',(-276.127908375746,229.181339034477,271.573593133701));
#19277=CARTESIAN_POINT('Origin',(-270.49584185083,116.321781057942,234.573593133701));
#19278=CARTESIAN_POINT('Origin',(-220.975944530184,177.305137423337,234.573593133701));
#19279=CARTESIAN_POINT('Origin',(-280.877471090321,173.835684387434,234.573593133701));
#19280=CARTESIAN_POINT('Origin',(-276.127908375746,229.181339034477,271.573593133701));
#19281=CARTESIAN_POINT('Origin',(-220.975944530184,177.305137423337,271.573593133701));
#19282=CARTESIAN_POINT('Origin',(-280.877471090321,173.835684387434,271.573593133701));
#19283=CARTESIAN_POINT('Origin',(-276.377114859149,234.175124785651,271.573593133701));
#19284=CARTESIAN_POINT('',(-276.377114859149,234.175124785651,271.573593133701));
#19285=CARTESIAN_POINT('',(-276.377114859149,234.175124785651,234.573593133701));
#19286=CARTESIAN_POINT('Origin',(-277.373940792763,254.150267790348,271.573593133701));
#19287=CARTESIAN_POINT('Origin',(-277.523464682805,257.146539241052,237.573593133701));
#19288=CARTESIAN_POINT('Origin',(-276.377114859149,234.175124785651,234.573593133701));
#19289=CARTESIAN_POINT('Origin',(-235.078442029538,259.264686746862,253.073593133701));
#19290=CARTESIAN_POINT('Origin',(-234.829235546134,254.270900995688,253.073593133701));
#19291=CARTESIAN_POINT('Origin',(-280.877471090321,173.835684387434,276.573593133701));
#19292=CARTESIAN_POINT('Origin',(-280.877471090321,173.835684387434,276.573593133701));
#19293=CARTESIAN_POINT('Origin',(-220.975944530184,177.305137423337,276.573593133701));
#19294=CARTESIAN_POINT('Origin',(-220.975944530184,177.305137423337,276.573593133701));
#19295=CARTESIAN_POINT('',(0.,0.,0.));
#19296=CARTESIAN_POINT('Origin',(-232.939627118415,176.278148255596,281.073593133703));
#19297=CARTESIAN_POINT('',(-224.957944681388,175.73708867065,280.073593133703));
#19298=CARTESIAN_POINT('Origin',(-232.939627118415,176.278148255596,280.073593133703));
#19299=CARTESIAN_POINT('',(-225.955654986017,175.804721118769,281.073593133703));
#19300=CARTESIAN_POINT('',(-225.955654986017,175.804721118769,281.073593133703));
#19301=CARTESIAN_POINT('Origin',(-232.939627118415,176.278148255596,281.073593133703));
#19302=CARTESIAN_POINT('Origin',(-232.939627118415,176.278148255596,226.073593133703));
#19303=CARTESIAN_POINT('',(-224.957944681388,175.73708867065,226.073593133703));
#19304=CARTESIAN_POINT('',(-240.921309555442,176.819207840542,226.073593133703));
#19305=CARTESIAN_POINT('Origin',(-232.939627118415,176.278148255596,226.073593133703));
#19306=CARTESIAN_POINT('Origin',(-232.939627118415,176.278148255596,226.073593133703));
#19307=CARTESIAN_POINT('',(-239.923599250813,176.751575392424,225.073593133703));
#19308=CARTESIAN_POINT('',(-240.921309555442,176.819207840542,226.073593133703));
#19309=CARTESIAN_POINT('Origin',(-232.939627118415,176.278148255596,225.073593133703));
#19310=CARTESIAN_POINT('Origin',(-232.939627118415,176.278148255596,281.073593133703));
#19311=CARTESIAN_POINT('',(-224.957944681388,175.73708867065,281.073593133703));
#19312=CARTESIAN_POINT('Origin',(-232.939627118415,176.278148255596,281.073593133703));
#19313=CARTESIAN_POINT('Origin',(-232.939627118415,176.278148255596,225.073593133703));
#19314=CARTESIAN_POINT('Origin',(-256.26210404747,132.050757761767,288.073593133703));
#19315=CARTESIAN_POINT('',(-248.262104896823,132.047071348801,287.073593133703));
#19316=CARTESIAN_POINT('Origin',(-256.26210404747,132.050757761767,287.073593133703));
#19317=CARTESIAN_POINT('',(-249.262104790654,132.047532150421,288.073593133703));
#19318=CARTESIAN_POINT('',(-249.262104790654,132.047532150421,288.073593133703));
#19319=CARTESIAN_POINT('Origin',(-256.26210404747,132.050757761767,288.073593133703));
#19320=CARTESIAN_POINT('Origin',(-256.26210404747,132.050757761767,219.073593133703));
#19321=CARTESIAN_POINT('',(-248.262104896823,132.047071348801,219.073593133703));
#19322=CARTESIAN_POINT('',(-264.262103198118,132.054444174733,219.073593133703));
#19323=CARTESIAN_POINT('Origin',(-256.26210404747,132.050757761767,219.073593133703));
#19324=CARTESIAN_POINT('Origin',(-256.26210404747,132.050757761767,219.073593133703));
#19325=CARTESIAN_POINT('',(-263.262103304287,132.053983373112,218.073593133703));
#19326=CARTESIAN_POINT('',(-264.262103198118,132.054444174733,219.073593133703));
#19327=CARTESIAN_POINT('Origin',(-256.26210404747,132.050757761767,218.073593133703));
#19328=CARTESIAN_POINT('Origin',(-256.26210404747,132.050757761767,288.073593133703));
#19329=CARTESIAN_POINT('',(-248.262104896823,132.047071348801,288.073593133703));
#19330=CARTESIAN_POINT('Origin',(-256.26210404747,132.050757761767,288.073593133703));
#19331=CARTESIAN_POINT('Origin',(-256.26210404747,132.050757761767,218.073593133703));
#19332=CARTESIAN_POINT('',(0.,0.,0.));
#19333=CARTESIAN_POINT('',(0.,0.,0.));
#19334=CARTESIAN_POINT('',(0.,0.,0.));
#19335=CARTESIAN_POINT('',(0.,0.,0.));
#19336=CARTESIAN_POINT('Origin',(-256.262104047423,132.050757761858,278.073593133703));
#19337=CARTESIAN_POINT('',(-264.241308724895,132.627206124688,278.073593133703));
#19338=CARTESIAN_POINT('Origin',(-256.262104047423,132.050757761858,278.073593133703));
#19339=CARTESIAN_POINT('',(-264.241308724895,132.627206124688,284.573593133703));
#19340=CARTESIAN_POINT('',(-264.241308724895,132.627206124688,278.073593133703));
#19341=CARTESIAN_POINT('Origin',(-256.262104047423,132.050757761858,284.573593133703));
#19342=CARTESIAN_POINT('Origin',(11.0412526478865,112.739737607035,278.073593133703));
#19343=CARTESIAN_POINT('',(3.06204797041458,113.316185969866,278.073593133703));
#19344=CARTESIAN_POINT('Origin',(11.0412526478865,112.739737607035,278.073593133703));
#19345=CARTESIAN_POINT('',(3.06204797041458,113.316185969866,284.573593133703));
#19346=CARTESIAN_POINT('',(3.06204797041458,113.316185969866,278.073593133703));
#19347=CARTESIAN_POINT('Origin',(11.0412526478865,112.739737607035,284.573593133703));
#19348=CARTESIAN_POINT('Origin',(-122.610425699768,122.395247684447,278.073593133703));
#19349=CARTESIAN_POINT('',(14.022070351669,98.487905240044,278.073593133703));
#19350=CARTESIAN_POINT('',(-261.260491021113,118.375373757697,278.073593133703));
#19351=CARTESIAN_POINT('',(23.9960761985089,97.7673447865059,278.073593133703));
#19352=CARTESIAN_POINT('',(-270.513936414414,129.069940058075,278.073593133703));
#19353=CARTESIAN_POINT('Origin',(-260.539930567575,128.349379604537,278.073593133703));
#19354=CARTESIAN_POINT('',(-269.937488051584,137.049144735547,278.073593133703));
#19355=CARTESIAN_POINT('',(-269.216927598046,147.023150582387,278.073593133703));
#19356=CARTESIAN_POINT('',(-259.242921751206,146.302590128849,278.073593133703));
#19357=CARTESIAN_POINT('Origin',(-259.963482204744,136.328584282009,278.073593133703));
#19358=CARTESIAN_POINT('',(16.0396396215758,126.415121611196,278.073593133703));
#19359=CARTESIAN_POINT('',(26.0136454684158,125.694561157658,278.073593133703));
#19360=CARTESIAN_POINT('',(25.2930850148776,115.720555310818,278.073593133703));
#19361=CARTESIAN_POINT('Origin',(15.3190791680377,116.441115764356,278.073593133703));
#19362=CARTESIAN_POINT('',(24.7166366520471,107.741350633346,278.073593133703));
#19363=CARTESIAN_POINT('',(26.0136454684158,125.694561157658,278.073593133703));
#19364=CARTESIAN_POINT('Origin',(14.7426308052072,108.461911086884,278.073593133703));
#19365=CARTESIAN_POINT('Origin',(-122.610425699768,122.395247684447,284.573593133703));
#19366=CARTESIAN_POINT('',(-270.513936414414,129.069940058075,284.573593133703));
#19367=CARTESIAN_POINT('',(-269.937488051584,137.049144735547,284.573593133703));
#19368=CARTESIAN_POINT('',(-269.216927598046,147.023150582387,284.573593133703));
#19369=CARTESIAN_POINT('',(-261.260491021113,118.375373757697,284.573593133703));
#19370=CARTESIAN_POINT('Origin',(-260.539930567575,128.349379604537,284.573593133703));
#19371=CARTESIAN_POINT('',(14.022070351669,98.487905240044,284.573593133703));
#19372=CARTESIAN_POINT('',(23.9960761985089,97.7673447865059,284.573593133703));
#19373=CARTESIAN_POINT('',(24.7166366520471,107.741350633346,284.573593133703));
#19374=CARTESIAN_POINT('Origin',(14.7426308052072,108.461911086884,284.573593133703));
#19375=CARTESIAN_POINT('',(25.2930850148776,115.720555310818,284.573593133703));
#19376=CARTESIAN_POINT('',(26.0136454684158,125.694561157658,284.573593133703));
#19377=CARTESIAN_POINT('',(16.0396396215758,126.415121611196,284.573593133703));
#19378=CARTESIAN_POINT('Origin',(15.3190791680377,116.441115764356,284.573593133703));
#19379=CARTESIAN_POINT('',(-259.242921751206,146.302590128849,284.573593133703));
#19380=CARTESIAN_POINT('',(26.0136454684158,125.694561157658,284.573593133703));
#19381=CARTESIAN_POINT('Origin',(-259.963482204744,136.328584282009,284.573593133703));
#19382=CARTESIAN_POINT('Origin',(-269.216927598046,147.023150582387,278.073593133703));
#19383=CARTESIAN_POINT('',(-270.513936414414,129.069940058075,278.073593133703));
#19384=CARTESIAN_POINT('',(-269.937488051584,137.049144735547,278.073593133703));
#19385=CARTESIAN_POINT('Origin',(26.0136454684158,125.694561157658,278.073593133703));
#19386=CARTESIAN_POINT('',(-259.242921751206,146.302590128849,278.073593133703));
#19387=CARTESIAN_POINT('',(16.0396396215758,126.415121611196,278.073593133703));
#19388=CARTESIAN_POINT('Origin',(26.0136454684158,125.694561157658,278.073593133703));
#19389=CARTESIAN_POINT('',(24.7166366520471,107.741350633346,278.073593133703));
#19390=CARTESIAN_POINT('',(25.2930850148776,115.720555310818,278.073593133703));
#19391=CARTESIAN_POINT('Origin',(23.9960761985089,97.7673447865059,278.073593133703));
#19392=CARTESIAN_POINT('',(-261.260491021113,118.375373757697,278.073593133703));
#19393=CARTESIAN_POINT('',(14.022070351669,98.487905240044,278.073593133703));
#19394=CARTESIAN_POINT('Origin',(-260.539930567575,128.349379604537,278.073593133703));
#19395=CARTESIAN_POINT('Origin',(-259.963482204744,136.328584282009,278.073593133703));
#19396=CARTESIAN_POINT('Origin',(14.7426308052072,108.461911086884,278.073593133703));
#19397=CARTESIAN_POINT('Origin',(15.3190791680377,116.441115764356,278.073593133703));
#19398=CARTESIAN_POINT('',(0.,0.,0.));
#19399=CARTESIAN_POINT('',(0.,0.,0.));
#19400=CARTESIAN_POINT('Origin',(290.197052756605,75.7062702018219,258.073593133703));
#19401=CARTESIAN_POINT('',(251.28301830691,84.6790771867611,258.573593133703));
#19402=CARTESIAN_POINT('',(251.850698433645,84.5481813729906,257.573593133703));
#19403=CARTESIAN_POINT('Ctrl Pts',(251.28301830691,84.6790771867611,258.573593133703));
#19404=CARTESIAN_POINT('Ctrl Pts',(251.268603243666,84.6165607113056,258.573593133703));
#19405=CARTESIAN_POINT('Ctrl Pts',(251.258879081903,84.5491576952367,258.560454544981));
#19406=CARTESIAN_POINT('Ctrl Pts',(251.253717921743,84.4239190897031,258.508711173615));
#19407=CARTESIAN_POINT('Ctrl Pts',(251.258359391243,84.3660629060774,258.4701484502));
#19408=CARTESIAN_POINT('Ctrl Pts',(251.279707190674,84.2692747335277,258.380631525734));
#19409=CARTESIAN_POINT('Ctrl Pts',(251.298791240693,84.2253450690978,258.322746863925));
#19410=CARTESIAN_POINT('Ctrl Pts',(251.350351032782,84.1622186524674,258.199249594304));
#19411=CARTESIAN_POINT('Ctrl Pts',(251.382858032475,84.1429364355382,258.133693745596));
#19412=CARTESIAN_POINT('Ctrl Pts',(251.451741110902,84.1270533595221,258.011254161343));
#19413=CARTESIAN_POINT('Ctrl Pts',(251.493650046494,84.1299802798894,257.945064916044));
#19414=CARTESIAN_POINT('Ctrl Pts',(251.581308030854,84.1614864113044,257.82231806015));
#19415=CARTESIAN_POINT('Ctrl Pts',(251.627007294045,84.1900499387627,257.765720879009));
#19416=CARTESIAN_POINT('Ctrl Pts',(251.706009704231,84.2617248254449,257.678127980836));
#19417=CARTESIAN_POINT('Ctrl Pts',(251.745188081272,84.3083492613558,257.639781389305));
#19418=CARTESIAN_POINT('Ctrl Pts',(251.810210027717,84.4193221435049,257.587468702232));
#19419=CARTESIAN_POINT('Ctrl Pts',(251.835859543139,84.4838268073212,257.573593133703));
#19420=CARTESIAN_POINT('Ctrl Pts',(251.850698433645,84.5481813729906,257.573593133703));
#19421=CARTESIAN_POINT('',(139.64640668573,110.42027268846,257.573593133703));
#19422=CARTESIAN_POINT('',(290.197052756605,75.7062702018219,257.573593133703));
#19423=CARTESIAN_POINT('Origin',(139.64640668573,110.42027268846,258.073593133703));
#19424=CARTESIAN_POINT('Ctrl Pts',(251.850698433645,84.5481813729906,257.573593133703));
#19425=CARTESIAN_POINT('Ctrl Pts',(251.864800464293,84.6093402619923,257.573593133703));
#19426=CARTESIAN_POINT('Ctrl Pts',(251.870281693377,84.6753901958754,257.586153033938));
#19427=CARTESIAN_POINT('Ctrl Pts',(251.86254067835,84.7986066327571,257.634024355935));
#19428=CARTESIAN_POINT('Ctrl Pts',(251.849537380392,84.8558232696689,257.669241832604));
#19429=CARTESIAN_POINT('Ctrl Pts',(251.812123690221,84.957939080529,257.754170475265));
#19430=CARTESIAN_POINT('Ctrl Pts',(251.782979802506,85.0070349671363,257.81235564874));
#19431=CARTESIAN_POINT('Ctrl Pts',(251.715900228166,85.0786514884424,257.93946956097));
#19432=CARTESIAN_POINT('Ctrl Pts',(251.678004374675,85.1011208931129,258.008448170203));
#19433=CARTESIAN_POINT('Ctrl Pts',(251.60659972071,85.1175853945944,258.135369851765));
#19434=CARTESIAN_POINT('Ctrl Pts',(251.567893496343,85.1140577619974,258.202697763481));
#19435=CARTESIAN_POINT('Ctrl Pts',(251.492031699182,85.0775518559062,258.329014288151));
#19436=CARTESIAN_POINT('Ctrl Pts',(251.4548040378,85.044514145115,258.387942404826));
#19437=CARTESIAN_POINT('Ctrl Pts',(251.393730641083,84.9644905748009,258.475703765116));
#19438=CARTESIAN_POINT('Ctrl Pts',(251.365353141457,84.9151907353916,258.512264506913));
#19439=CARTESIAN_POINT('Ctrl Pts',(251.31702147063,84.8027912190808,258.561229944453));
#19440=CARTESIAN_POINT('Ctrl Pts',(251.296997530561,84.7397034759105,258.573593133703));
#19441=CARTESIAN_POINT('Ctrl Pts',(251.28301830691,84.6790771867611,258.573593133703));
#19442=CARTESIAN_POINT('Origin',(277.041252647849,78.7397376070303,227.073593133703));
#19443=CARTESIAN_POINT('',(288.247215261781,76.155864178403,225.073593133703));
#19444=CARTESIAN_POINT('Origin',(277.041252647849,78.7397376070303,225.073593133703));
#19445=CARTESIAN_POINT('',(290.196078325073,75.7064948864679,227.073593133703));
#19446=CARTESIAN_POINT('Origin',(288.247215261781,76.155864178403,227.073593133703));
#19447=CARTESIAN_POINT('',(263.886426970625,81.7729803275927,227.073593133703));
#19448=CARTESIAN_POINT('Origin',(277.041252647849,78.7397376070303,227.073593133703));
#19449=CARTESIAN_POINT('Origin',(277.041252647849,78.7397376070303,227.073593133703));
#19450=CARTESIAN_POINT('Origin',(277.041252647849,78.7397376070303,279.073593133703));
#19451=CARTESIAN_POINT('',(263.886426970625,81.7729803275927,279.073593133703));
#19452=CARTESIAN_POINT('',(290.196078325073,75.7064948864678,279.073593133703));
#19453=CARTESIAN_POINT('Origin',(277.041252647849,78.7397376070303,279.073593133703));
#19454=CARTESIAN_POINT('Origin',(277.041252647849,78.7397376070303,279.073593133703));
#19455=CARTESIAN_POINT('',(288.247215261781,76.155864178403,281.073593133703));
#19456=CARTESIAN_POINT('Origin',(288.247215261781,76.155864178403,279.073593133703));
#19457=CARTESIAN_POINT('Origin',(277.041252647849,78.7397376070303,281.073593133703));
#19458=CARTESIAN_POINT('Origin',(139.64640668573,110.42027268846,253.073593133703));
#19459=CARTESIAN_POINT('',(139.64640668573,110.42027268846,245.573593133703));
#19460=CARTESIAN_POINT('Origin',(139.64640668573,110.42027268846,253.073593133703));
#19461=CARTESIAN_POINT('',(125.029933711037,113.790542377974,245.573593133703));
#19462=CARTESIAN_POINT('',(139.64640668573,110.42027268846,245.573593133703));
#19463=CARTESIAN_POINT('Origin',(125.029933711037,113.790542377974,253.073593133703));
#19464=CARTESIAN_POINT('Origin',(255.074370622327,80.7261481941816,260.573593133704));
#19465=CARTESIAN_POINT('',(255.074370622327,80.7261481941816,265.573593133704));
#19466=CARTESIAN_POINT('Origin',(255.074370622327,80.7261481941816,260.573593133704));
#19467=CARTESIAN_POINT('',(264.061756461031,119.703409460031,265.573593133704));
#19468=CARTESIAN_POINT('',(255.074370622327,80.7261481941816,265.573593133704));
#19469=CARTESIAN_POINT('Origin',(264.061756461031,119.703409460031,260.573593133704));
#19470=CARTESIAN_POINT('Origin',(239.288983046701,153.123984191655,281.073593133703));
#19471=CARTESIAN_POINT('',(243.430317056198,152.169074446293,269.073593133703));
#19472=CARTESIAN_POINT('Origin',(239.288983046701,153.123984191655,269.073593133703));
#19473=CARTESIAN_POINT('',(243.430317056198,152.169074446293,251.073593133703));
#19474=CARTESIAN_POINT('',(243.430317056198,152.169074446293,281.073593133703));
#19475=CARTESIAN_POINT('Origin',(239.288983046701,153.123984191655,251.073593133703));
#19476=CARTESIAN_POINT('Origin',(277.041252647849,78.7397376070303,281.073593133703));
#19477=CARTESIAN_POINT('',(284.836704901019,76.9422604392896,281.073593133703));
#19478=CARTESIAN_POINT('Origin',(277.041252647849,78.7397376070303,281.073593133703));
#19479=CARTESIAN_POINT('',(284.836704901019,76.9422604392896,225.073593133703));
#19480=CARTESIAN_POINT('',(284.836704901019,76.9422604392896,281.073593133703));
#19481=CARTESIAN_POINT('Origin',(277.041252647849,78.7397376070303,225.073593133703));
#19482=CARTESIAN_POINT('Origin',(261.812330085074,110.608660518952,263.143363115103));
#19483=CARTESIAN_POINT('',(260.506630277985,120.523151270375,266.635682465084));
#19484=CARTESIAN_POINT('',(267.32755142688,118.950381708081,266.635682465084));
#19485=CARTESIAN_POINT('Origin',(263.917090852633,119.73676648918,252.326565285529));
#19486=CARTESIAN_POINT('',(260.455987287139,120.461895956422,266.697317490661));
#19487=CARTESIAN_POINT('Origin',(262.326343033394,112.718291331958,260.527055021389));
#19488=CARTESIAN_POINT('',(260.359612810304,120.043930907366,267.192605719228));
#19489=CARTESIAN_POINT('',(261.400356029357,124.557514844643,261.84401258248));
#19490=CARTESIAN_POINT('',(263.599526276829,118.359525358802,269.233847171548));
#19491=CARTESIAN_POINT('Origin',(260.627227793702,105.469007847775,269.233847171476));
#19492=CARTESIAN_POINT('',(267.249884248594,118.455170539444,267.192605719228));
#19493=CARTESIAN_POINT('Origin',(260.62722779321,105.469007845778,269.23384717163));
#19494=CARTESIAN_POINT('',(267.346258725429,118.8731355885,266.697317490661));
#19495=CARTESIAN_POINT('',(266.846226172141,116.704551773281,269.267087472061));
#19496=CARTESIAN_POINT('Origin',(262.311555516519,112.776310611233,260.572594253834));
#19497=CARTESIAN_POINT('Origin',(261.395367346685,108.800340960407,255.860966009446));
#19498=CARTESIAN_POINT('',(263.599526276829,118.359525358802,251.913339095859));
#19499=CARTESIAN_POINT('',(267.249884248594,118.455170539444,253.954580548178));
#19500=CARTESIAN_POINT('Origin',(260.62722779329,105.469007845961,251.913339095793));
#19501=CARTESIAN_POINT('',(260.359612810304,120.043930907366,253.954580548178));
#19502=CARTESIAN_POINT('Origin',(260.627227793615,105.469007846882,251.913339095865));
#19503=CARTESIAN_POINT('',(260.455987287139,120.461895956422,254.449868776745));
#19504=CARTESIAN_POINT('',(260.983393290967,122.749195286098,257.160316542069));
#19505=CARTESIAN_POINT('',(260.506630277985,120.523151270375,254.511503802322));
#19506=CARTESIAN_POINT('Origin',(262.319364171497,112.747732317274,260.596894987617));
#19507=CARTESIAN_POINT('',(267.32755142688,118.950381708081,254.511503802323));
#19508=CARTESIAN_POINT('Origin',(263.917090852491,119.736766489213,268.820620983067));
#19509=CARTESIAN_POINT('',(267.346258725429,118.8731355885,254.449868776745));
#19510=CARTESIAN_POINT('Origin',(262.33579074407,112.805792616964,260.54516207062));
#19511=CARTESIAN_POINT('',(266.429263433752,114.896232214736,249.737241652488));
#19512=CARTESIAN_POINT('Origin',(260.546821162919,105.120293514534,260.573593133703));
#19513=CARTESIAN_POINT('',(265.60821119059,93.6908433533151,260.573593133703));
#19514=CARTESIAN_POINT('Origin',(258.299974703243,95.375978198072,260.573593133703));
#19515=CARTESIAN_POINT('',(267.855057650266,103.435158669777,260.573593133703));
#19516=CARTESIAN_POINT('',(267.855057650266,103.435158669777,260.573593133703));
#19517=CARTESIAN_POINT('',(264.200939406592,104.277726092156,267.068783662087));
#19518=CARTESIAN_POINT('Origin',(260.546821162919,105.120293514534,260.573593133703));
#19519=CARTESIAN_POINT('',(256.892702919245,105.962860936913,267.068783662087));
#19520=CARTESIAN_POINT('Origin',(260.546821162919,105.120293514534,260.573593133703));
#19521=CARTESIAN_POINT('',(253.238584675572,106.805428359291,260.573593133703));
#19522=CARTESIAN_POINT('Origin',(260.546821162919,105.120293514534,260.573593133703));
#19523=CARTESIAN_POINT('',(256.892702919245,105.962860936913,254.07840260532));
#19524=CARTESIAN_POINT('Origin',(260.546821162919,105.120293514534,260.573593133703));
#19525=CARTESIAN_POINT('',(264.200939406592,104.277726092156,254.07840260532));
#19526=CARTESIAN_POINT('Origin',(260.546821162919,105.120293514534,260.573593133703));
#19527=CARTESIAN_POINT('Origin',(260.546821162919,105.120293514534,260.573593133703));
#19528=CARTESIAN_POINT('Origin',(244.644544516272,152.915336968997,253.073593133703));
#19529=CARTESIAN_POINT('',(246.891390975948,162.65965228546,251.073593133703));
#19530=CARTESIAN_POINT('',(254.062847596205,149.554449125806,251.073593133703));
#19531=CARTESIAN_POINT('Origin',(244.644544516272,152.915336968997,251.073593133703));
#19532=CARTESIAN_POINT('',(246.891390975948,162.65965228546,269.073593133703));
#19533=CARTESIAN_POINT('',(246.891390975948,162.65965228546,251.073593133703));
#19534=CARTESIAN_POINT('',(254.062847596205,149.554449125806,269.073593133703));
#19535=CARTESIAN_POINT('Origin',(244.644544516272,152.915336968997,269.073593133703));
#19536=CARTESIAN_POINT('',(254.062847596205,149.554449125806,269.073593133703));
#19537=CARTESIAN_POINT('Origin',(131.363738666737,112.330092179185,253.073593133703));
#19538=CARTESIAN_POINT('',(126.195991809483,89.9181669513215,253.073593133703));
#19539=CARTESIAN_POINT('Origin',(131.363738666737,112.330092179185,253.073593133703));
#19540=CARTESIAN_POINT('',(131.068149467714,88.7947437214835,253.073593133703));
#19541=CARTESIAN_POINT('',(126.195991809483,89.9181669513215,253.073593133703));
#19542=CARTESIAN_POINT('Origin',(136.235896324969,111.206668949347,253.073593133703));
#19543=CARTESIAN_POINT('Origin',(131.363738666737,112.330092179185,253.073593133703));
#19544=CARTESIAN_POINT('',(130.95580714473,88.3075279556604,253.073593133703));
#19545=CARTESIAN_POINT('Origin',(136.235896324969,111.206668949347,253.073593133703));
#19546=CARTESIAN_POINT('',(131.930238676376,88.0828433096928,253.073593133703));
#19547=CARTESIAN_POINT('',(126.083649486499,89.4309511854984,253.073593133703));
#19548=CARTESIAN_POINT('Origin',(137.210327856615,110.981984303379,253.073593133703));
#19549=CARTESIAN_POINT('Origin',(131.363738666737,112.330092179185,253.073593133703));
#19550=CARTESIAN_POINT('',(131.593211707425,86.6211960122235,253.073593133703));
#19551=CARTESIAN_POINT('Origin',(137.210327856615,110.981984303379,253.073593133703));
#19552=CARTESIAN_POINT('',(209.547734239124,68.6464243348164,253.073593133703));
#19553=CARTESIAN_POINT('',(125.746622517548,87.969303888029,253.073593133703));
#19554=CARTESIAN_POINT('Origin',(215.164850388313,93.0072126259722,253.073593133703));
#19555=CARTESIAN_POINT('Origin',(131.363738666737,112.330092179185,253.073593133703));
#19556=CARTESIAN_POINT('',(209.098364947188,66.6975612715239,253.073593133703));
#19557=CARTESIAN_POINT('Origin',(215.164850388313,93.0072126259722,253.073593133703));
#19558=CARTESIAN_POINT('',(210.560012244658,66.3605343025725,253.073593133703));
#19559=CARTESIAN_POINT('',(125.297253225612,86.0204408247366,253.073593133703));
#19560=CARTESIAN_POINT('',(221.513065902147,113.862671378776,269.073593133703));
#19561=CARTESIAN_POINT('Origin',(216.626497685783,92.6701856570208,253.073593133703));
#19562=CARTESIAN_POINT('',(222.676316926623,118.907557612938,251.073593133703));
#19563=CARTESIAN_POINT('Origin',(216.626497685783,92.6701856570208,253.073593133703));
#19564=CARTESIAN_POINT('Origin',(216.626497685783,92.6701856570208,253.073593133703));
#19565=CARTESIAN_POINT('Origin',(216.626497685783,92.6701856570208,253.073593133703));
#19566=CARTESIAN_POINT('',(240.538123974849,111.65376571076,251.073593133703));
#19567=CARTESIAN_POINT('',(238.543161711281,106.063231272255,269.073593133703));
#19568=CARTESIAN_POINT('Origin',(232.30684086269,88.5870277819392,253.073593133703));
#19569=CARTESIAN_POINT('Ctrl Pts',(238.543161711281,106.063231272255,269.073593133703));
#19570=CARTESIAN_POINT('Ctrl Pts',(230.852920983076,109.661454372805,269.073593133703));
#19571=CARTESIAN_POINT('Ctrl Pts',(221.513065902155,113.862671378773,269.073593133703));
#19572=CARTESIAN_POINT('',(235.819539119684,64.6411442799677,253.073593133703));
#19573=CARTESIAN_POINT('',(210.560012244658,66.3605343025725,253.073593133703));
#19574=CARTESIAN_POINT('',(240.249036425902,83.8513659038506,275.837689461751));
#19575=CARTESIAN_POINT('Origin',(240.987285976938,87.0530695078311,253.073593133703));
#19576=CARTESIAN_POINT('',(243.448117813726,97.7254148544326,273.29846276181));
#19577=CARTESIAN_POINT('Origin',(240.987285976938,87.0530695078311,253.073593133703));
#19578=CARTESIAN_POINT('',(243.448117813726,97.7254148544326,232.848723505596));
#19579=CARTESIAN_POINT('Origin',(240.987285976938,87.0530695078311,253.073593133703));
#19580=CARTESIAN_POINT('',(240.249036425902,83.8513659038506,230.309496805655));
#19581=CARTESIAN_POINT('Origin',(240.987285976938,87.0530695078311,253.073593133703));
#19582=CARTESIAN_POINT('Origin',(240.987285976938,87.0530695078311,253.073593133703));
#19583=CARTESIAN_POINT('Ctrl Pts',(222.676316926623,118.907557612938,251.073593133703));
#19584=CARTESIAN_POINT('Ctrl Pts',(228.630385342599,116.489953848209,251.073593133703));
#19585=CARTESIAN_POINT('Ctrl Pts',(234.584338031647,114.07206503216,251.073593133703));
#19586=CARTESIAN_POINT('Ctrl Pts',(240.538123974849,111.65376571076,251.073593133703));
#19587=CARTESIAN_POINT('Origin',(277.041252647849,78.7397376070303,225.073593133703));
#19588=CARTESIAN_POINT('',(263.886426970625,81.7729803275927,278.073593133703));
#19589=CARTESIAN_POINT('',(263.886426970625,81.7729803275927,225.073593133703));
#19590=CARTESIAN_POINT('',(263.544486310321,78.4442745295379,277.78120466771));
#19591=CARTESIAN_POINT('Ctrl Pts',(263.886446492733,81.7729758257347,278.073577619317));
#19592=CARTESIAN_POINT('Ctrl Pts',(263.85275455139,81.6268667898238,278.073579192226));
#19593=CARTESIAN_POINT('Ctrl Pts',(263.821493169456,81.4802343246266,278.071810719886));
#19594=CARTESIAN_POINT('Ctrl Pts',(263.792761752791,81.333477957104,278.068267543646));
#19595=CARTESIAN_POINT('Ctrl Pts',(263.752444668704,81.1275434959372,278.063295615668));
#19596=CARTESIAN_POINT('Ctrl Pts',(263.716974024298,80.9209501746423,278.054856597271));
#19597=CARTESIAN_POINT('Ctrl Pts',(263.686312053167,80.7134721297003,278.042963391396));
#19598=CARTESIAN_POINT('Ctrl Pts',(263.669333854775,80.5985870365692,278.036377865371));
#19599=CARTESIAN_POINT('Ctrl Pts',(263.653830777329,80.4834305611799,278.028732724067));
#19600=CARTESIAN_POINT('Ctrl Pts',(263.639801959899,80.3679634694504,278.020026203797));
#19601=CARTESIAN_POINT('Ctrl Pts',(263.629457986628,80.2828252518821,278.013606559846));
#19602=CARTESIAN_POINT('Ctrl Pts',(263.619941007641,80.1977065301477,278.006621309609));
#19603=CARTESIAN_POINT('Ctrl Pts',(263.61124379958,80.1126083918287,277.999079084841));
#19604=CARTESIAN_POINT('Ctrl Pts',(263.590437455768,79.9090279886416,277.981035809284));
#19605=CARTESIAN_POINT('Ctrl Pts',(263.57432785594,79.7056452709986,277.959809986454));
#19606=CARTESIAN_POINT('Ctrl Pts',(263.562830679749,79.5024395682177,277.935503430205));
#19607=CARTESIAN_POINT('Ctrl Pts',(263.551203283478,79.2969323035088,277.910921571423));
#19608=CARTESIAN_POINT('Ctrl Pts',(263.544293467851,79.0916056610182,277.883188588102));
#19609=CARTESIAN_POINT('Ctrl Pts',(263.542058389097,78.8864524133771,277.852383645832));
#19610=CARTESIAN_POINT('Ctrl Pts',(263.540451601139,78.7389686760395,277.830238112839));
#19611=CARTESIAN_POINT('Ctrl Pts',(263.541261700963,78.5915748264037,277.806504400391));
#19612=CARTESIAN_POINT('Ctrl Pts',(263.544486310321,78.4442745295379,277.78120466771));
#19613=CARTESIAN_POINT('',(264.697446773203,73.2734363904916,272.907655056344));
#19614=CARTESIAN_POINT('Ctrl Pts',(263.544486310321,78.4442745295379,277.78120466771));
#19615=CARTESIAN_POINT('Ctrl Pts',(263.547122992337,78.3238307793806,277.760517709776));
#19616=CARTESIAN_POINT('Ctrl Pts',(263.551293306596,78.205570043004,277.73432802133));
#19617=CARTESIAN_POINT('Ctrl Pts',(263.556873433881,78.0893078590764,277.703178796516));
#19618=CARTESIAN_POINT('Ctrl Pts',(263.5624795862,77.9725034424917,277.671884295515));
#19619=CARTESIAN_POINT('Ctrl Pts',(263.569508560945,77.8577154073319,277.635584233554));
#19620=CARTESIAN_POINT('Ctrl Pts',(263.5778464509,77.7447342870386,277.594783472228));
#19621=CARTESIAN_POINT('Ctrl Pts',(263.582583675622,77.6805433515511,277.57160226256));
#19622=CARTESIAN_POINT('Ctrl Pts',(263.587743651842,77.6169353572849,277.546967348406));
#19623=CARTESIAN_POINT('Ctrl Pts',(263.593307356281,77.5538702101861,277.52096425551));
#19624=CARTESIAN_POINT('Ctrl Pts',(263.603116432212,77.4426833519792,277.475119564176));
#19625=CARTESIAN_POINT('Ctrl Pts',(263.614188157078,77.3331122049833,277.424934853952));
#19626=CARTESIAN_POINT('Ctrl Pts',(263.626398085071,77.2251933445278,277.370779250483));
#19627=CARTESIAN_POINT('Ctrl Pts',(263.639089736436,77.1130167163494,277.314487023449));
#19628=CARTESIAN_POINT('Ctrl Pts',(263.653011113268,77.0026258188698,277.253904489932));
#19629=CARTESIAN_POINT('Ctrl Pts',(263.668008001099,76.8940658959719,277.189500756005));
#19630=CARTESIAN_POINT('Ctrl Pts',(263.672343279029,76.8626835556453,277.170883020818));
#19631=CARTESIAN_POINT('Ctrl Pts',(263.676768348929,76.8314542219291,277.151946290177));
#19632=CARTESIAN_POINT('Ctrl Pts',(263.681279292772,76.8003789551962,277.132702662197));
#19633=CARTESIAN_POINT('Ctrl Pts',(263.684570894048,76.7777035703618,277.11866073381));
#19634=CARTESIAN_POINT('Ctrl Pts',(263.68790110023,76.755157409625,277.10448259259));
#19635=CARTESIAN_POINT('Ctrl Pts',(263.691268503701,76.732740170163,277.090171883745));
#19636=CARTESIAN_POINT('Ctrl Pts',(263.709908083934,76.6086540791465,277.010957851916));
#19637=CARTESIAN_POINT('Ctrl Pts',(263.729710767152,76.4883513320883,276.927778617926));
#19638=CARTESIAN_POINT('Ctrl Pts',(263.750512514209,76.3714290619651,276.841087289969));
#19639=CARTESIAN_POINT('Ctrl Pts',(263.771934050831,76.25102308431,276.751812987597));
#19640=CARTESIAN_POINT('Ctrl Pts',(263.794415147851,76.1342022342419,276.658813972525));
#19641=CARTESIAN_POINT('Ctrl Pts',(263.817791248369,76.0205596546528,276.562540155481));
#19642=CARTESIAN_POINT('Ctrl Pts',(263.842448812904,75.9006872560012,276.460988664675));
#19643=CARTESIAN_POINT('Ctrl Pts',(263.86810223401,75.7843512561059,276.355793378961));
#19644=CARTESIAN_POINT('Ctrl Pts',(263.894573572594,75.6711080942386,276.247435360569));
#19645=CARTESIAN_POINT('Ctrl Pts',(263.916073581254,75.5791320518042,276.159427029352));
#19646=CARTESIAN_POINT('Ctrl Pts',(263.938113471031,75.4891969946826,276.069331328785));
#19647=CARTESIAN_POINT('Ctrl Pts',(263.960604308298,75.4010793409905,275.977386216045));
#19648=CARTESIAN_POINT('Ctrl Pts',(263.966186804265,75.3792074808841,275.954564334628));
#19649=CARTESIAN_POINT('Ctrl Pts',(263.971800969941,75.3574410130864,275.931613553638));
#19650=CARTESIAN_POINT('Ctrl Pts',(263.977445212981,75.3357801371126,275.90853904003));
#19651=CARTESIAN_POINT('Ctrl Pts',(264.012422701034,75.2015472514492,275.765545813408));
#19652=CARTESIAN_POINT('Ctrl Pts',(264.048568414587,75.0713158394443,275.617760857594));
#19653=CARTESIAN_POINT('Ctrl Pts',(264.085470719744,74.9453104927299,275.466568118245));
#19654=CARTESIAN_POINT('Ctrl Pts',(264.100639812602,74.8935146280335,275.404418702568));
#19655=CARTESIAN_POINT('Ctrl Pts',(264.115936918988,74.8424326620172,275.341692923535));
#19656=CARTESIAN_POINT('Ctrl Pts',(264.131334181614,74.7920794157389,275.278484566265));
#19657=CARTESIAN_POINT('Ctrl Pts',(264.136682122934,74.7745901897056,275.256530366105));
#19658=CARTESIAN_POINT('Ctrl Pts',(264.142041182813,74.7571908096217,275.234521931448));
#19659=CARTESIAN_POINT('Ctrl Pts',(264.147410915155,74.7398797847651,275.212460526197));
#19660=CARTESIAN_POINT('Ctrl Pts',(264.191265460638,74.5985008335307,275.032285270083));
#19661=CARTESIAN_POINT('Ctrl Pts',(264.235856933395,74.4629273361703,274.848488464814));
#19662=CARTESIAN_POINT('Ctrl Pts',(264.280980144503,74.3323009810995,274.661588044547));
#19663=CARTESIAN_POINT('Ctrl Pts',(264.291813083473,74.3009409050408,274.616717992161));
#19664=CARTESIAN_POINT('Ctrl Pts',(264.302676726821,74.2698661512641,274.571668927922));
#19665=CARTESIAN_POINT('Ctrl Pts',(264.313568343616,74.2390651848461,274.526447774819));
#19666=CARTESIAN_POINT('Ctrl Pts',(264.317765143417,74.2271968376442,274.509022985654));
#19667=CARTESIAN_POINT('Ctrl Pts',(264.32196588765,74.2153690830843,274.491572522455));
#19668=CARTESIAN_POINT('Ctrl Pts',(264.326170501729,74.2035814297529,274.474096678514));
#19669=CARTESIAN_POINT('Ctrl Pts',(264.369955565245,74.0808298192456,274.29211066922));
#19670=CARTESIAN_POINT('Ctrl Pts',(264.414158406344,73.9624286077785,274.107379181318));
#19671=CARTESIAN_POINT('Ctrl Pts',(264.458698703332,73.8478348019593,273.920240767794));
#19672=CARTESIAN_POINT('Ctrl Pts',(264.475771742853,73.803909082825,273.848507489255));
#19673=CARTESIAN_POINT('Ctrl Pts',(264.492894372165,73.7605432081688,273.776420191835));
#19674=CARTESIAN_POINT('Ctrl Pts',(264.510062044817,73.7177081324413,273.703996648076));
#19675=CARTESIAN_POINT('Ctrl Pts',(264.541713431899,73.6387347276007,273.570472106702));
#19676=CARTESIAN_POINT('Ctrl Pts',(264.573627236761,73.5613001852101,273.435322169166));
#19677=CARTESIAN_POINT('Ctrl Pts',(264.605605641687,73.4856481451905,273.299400074616));
#19678=CARTESIAN_POINT('Ctrl Pts',(264.636222180717,73.4132179023013,273.169266500958));
#19679=CARTESIAN_POINT('Ctrl Pts',(264.66689779028,73.342420324327,273.038425986335));
#19680=CARTESIAN_POINT('Ctrl Pts',(264.697446430188,73.2734364754757,272.907654931384));
#19681=CARTESIAN_POINT('',(264.697446773204,73.273436390491,233.239531211061));
#19682=CARTESIAN_POINT('',(264.697446473732,73.2734363771458,281.073593133703));
#19683=CARTESIAN_POINT('',(263.544486310321,78.4442745295379,228.365981599697));
#19684=CARTESIAN_POINT('Ctrl Pts',(264.697446430188,73.2734364754763,233.239531336022));
#19685=CARTESIAN_POINT('Ctrl Pts',(264.663254910726,73.3506465449807,233.093166028613));
#19686=CARTESIAN_POINT('Ctrl Pts',(264.62902021271,73.4298652314763,232.947195179886));
#19687=CARTESIAN_POINT('Ctrl Pts',(264.594902967084,73.5110401054218,232.802302791382));
#19688=CARTESIAN_POINT('Ctrl Pts',(264.566508978667,73.5785976818973,232.681716480109));
#19689=CARTESIAN_POINT('Ctrl Pts',(264.538196350838,73.647509921883,232.561876938124));
#19690=CARTESIAN_POINT('Ctrl Pts',(264.510055257259,73.7177250681167,232.443160985242));
#19691=CARTESIAN_POINT('Ctrl Pts',(264.465269218582,73.8294711964643,232.254226705116));
#19692=CARTESIAN_POINT('Ctrl Pts',(264.420789806233,73.9448269326336,232.067578466915));
#19693=CARTESIAN_POINT('Ctrl Pts',(264.376697369361,74.0643200580235,231.883541793551));
#19694=CARTESIAN_POINT('Ctrl Pts',(264.35979481214,74.1101269930158,231.812992497049));
#19695=CARTESIAN_POINT('Ctrl Pts',(264.342949112854,74.1565423392094,231.742827319498));
#19696=CARTESIAN_POINT('Ctrl Pts',(264.326164814146,74.2035973749484,231.673065948251));
#19697=CARTESIAN_POINT('Ctrl Pts',(264.321962099464,74.2153797492373,231.655598007274));
#19698=CARTESIAN_POINT('Ctrl Pts',(264.317763251177,74.227202188807,231.638155424292));
#19699=CARTESIAN_POINT('Ctrl Pts',(264.313568343771,74.2390651844082,231.620738492203));
#19700=CARTESIAN_POINT('Ctrl Pts',(264.268201373635,74.3673607854903,231.432378330354));
#19701=CARTESIAN_POINT('Ctrl Pts',(264.223318747672,74.5004034612182,231.247001665634));
#19702=CARTESIAN_POINT('Ctrl Pts',(264.179122612568,74.6390415540256,231.065119437598));
#19703=CARTESIAN_POINT('Ctrl Pts',(264.168509912247,74.6723323503493,231.02144454215));
#19704=CARTESIAN_POINT('Ctrl Pts',(264.157936852948,74.705945969639,230.977971270434));
#19705=CARTESIAN_POINT('Ctrl Pts',(264.147406342131,74.7398945273785,230.934706951834));
#19706=CARTESIAN_POINT('Ctrl Pts',(264.142038140199,74.7572006881552,230.912651839528));
#19707=CARTESIAN_POINT('Ctrl Pts',(264.136680604834,74.774595154308,230.890649668241));
#19708=CARTESIAN_POINT('Ctrl Pts',(264.131334181738,74.7920794153349,230.868701700738));
#19709=CARTESIAN_POINT('Ctrl Pts',(264.093877580934,74.9145727110991,230.714936044264));
#19710=CARTESIAN_POINT('Ctrl Pts',(264.057012652599,75.0413796191397,230.56402291816));
#19711=CARTESIAN_POINT('Ctrl Pts',(264.021144891591,75.1722820846851,230.417326682335));
#19712=CARTESIAN_POINT('Ctrl Pts',(264.006398845075,75.2260990443088,230.357016547095));
#19713=CARTESIAN_POINT('Ctrl Pts',(263.991821517935,75.2806080558477,230.29741972076));
#19714=CARTESIAN_POINT('Ctrl Pts',(263.977441810656,75.3357931942203,230.238633316917));
#19715=CARTESIAN_POINT('Ctrl Pts',(263.971798713818,75.3574497602277,230.215563489193));
#19716=CARTESIAN_POINT('Ctrl Pts',(263.966185682656,75.3792118752832,230.192617345688));
#19717=CARTESIAN_POINT('Ctrl Pts',(263.960604308547,75.4010793400128,230.169800050216));
#19718=CARTESIAN_POINT('Ctrl Pts',(263.93293244652,75.5094959154173,230.05667431453));
#19719=CARTESIAN_POINT('Ctrl Pts',(263.905942876101,75.6206628873982,229.946347126665));
#19720=CARTESIAN_POINT('Ctrl Pts',(263.879802393058,75.7349992059669,229.839265251712));
#19721=CARTESIAN_POINT('Ctrl Pts',(263.854558246421,75.8454150229674,229.735855129217));
#19722=CARTESIAN_POINT('Ctrl Pts',(263.830105880425,75.9587863617574,229.63547133516));
#19723=CARTESIAN_POINT('Ctrl Pts',(263.806607422103,76.0755167676874,229.538553045713));
#19724=CARTESIAN_POINT('Ctrl Pts',(263.784247108639,76.1865933511585,229.446328981367));
#19725=CARTESIAN_POINT('Ctrl Pts',(263.762750505002,76.3007113943396,229.357242760094));
#19726=CARTESIAN_POINT('Ctrl Pts',(263.742268982999,76.41824476033,229.271708885874));
#19727=CARTESIAN_POINT('Ctrl Pts',(263.724465455108,76.5204104372433,229.197358712329));
#19728=CARTESIAN_POINT('Ctrl Pts',(263.707429038303,76.6251569658246,229.1256930543));
#19729=CARTESIAN_POINT('Ctrl Pts',(263.691267273814,76.7327483577029,229.057009150204));
#19730=CARTESIAN_POINT('Ctrl Pts',(263.687900289533,76.7551628982351,229.042700215954));
#19731=CARTESIAN_POINT('Ctrl Pts',(263.684570493643,76.7777063287377,229.028523817602));
#19732=CARTESIAN_POINT('Ctrl Pts',(263.681279293248,76.8003789519183,229.014483599006));
#19733=CARTESIAN_POINT('Ctrl Pts',(263.665616777329,76.9082758524226,228.94766750733));
#19734=CARTESIAN_POINT('Ctrl Pts',(263.650990460361,77.0180303308622,228.88455500451));
#19735=CARTESIAN_POINT('Ctrl Pts',(263.637560028327,77.1295969108204,228.825635123568));
#19736=CARTESIAN_POINT('Ctrl Pts',(263.624663225137,77.2367306367194,228.769056295237));
#19737=CARTESIAN_POINT('Ctrl Pts',(263.612869251473,77.345534854029,228.716343689266));
#19738=CARTESIAN_POINT('Ctrl Pts',(263.602307206215,77.4559709595898,228.667883260715));
#19739=CARTESIAN_POINT('Ctrl Pts',(263.599199542263,77.4884645056732,228.653624779213));
#19740=CARTESIAN_POINT('Ctrl Pts',(263.596198439943,77.5210993620194,228.639734085692));
#19741=CARTESIAN_POINT('Ctrl Pts',(263.593306963389,77.5538746636589,228.626220175638));
#19742=CARTESIAN_POINT('Ctrl Pts',(263.583514536842,77.6648732237023,228.58045325721));
#19743=CARTESIAN_POINT('Ctrl Pts',(263.5749720485,77.7775539423449,228.538921908102));
#19744=CARTESIAN_POINT('Ctrl Pts',(263.567786046187,77.8921334806293,228.502103165652));
#19745=CARTESIAN_POINT('Ctrl Pts',(263.560624490531,78.0063232212909,228.465409679932));
#19746=CARTESIAN_POINT('Ctrl Pts',(263.554810288292,78.1223996733709,228.433397020835));
#19747=CARTESIAN_POINT('Ctrl Pts',(263.550461447433,78.2405621917892,228.406585073276));
#19748=CARTESIAN_POINT('Ctrl Pts',(263.547987548257,78.3077805992609,228.391332720497));
#19749=CARTESIAN_POINT('Ctrl Pts',(263.545988077553,78.3756737364794,228.377764209574));
#19750=CARTESIAN_POINT('Ctrl Pts',(263.544486310321,78.4442745295379,228.365981599697));
#19751=CARTESIAN_POINT('',(263.886426970624,81.772980327589,228.073593133703));
#19752=CARTESIAN_POINT('Ctrl Pts',(263.544486310321,78.4442745295379,228.365981599697));
#19753=CARTESIAN_POINT('Ctrl Pts',(263.532233262231,79.0039943036223,228.269846283192));
#19754=CARTESIAN_POINT('Ctrl Pts',(263.554916335949,79.564270344569,228.1964953478));
#19755=CARTESIAN_POINT('Ctrl Pts',(263.668901959567,80.6739967475123,228.098538799407));
#19756=CARTESIAN_POINT('Ctrl Pts',(263.760142632711,81.2252996425734,228.073593133703));
#19757=CARTESIAN_POINT('Ctrl Pts',(263.886426970624,81.772980327589,228.073593133703));
#19758=CARTESIAN_POINT('',(263.886426970625,81.7729803275927,225.073593133703));
#19759=CARTESIAN_POINT('',(270.946701599761,90.7857513677001,231.090039190109));
#19760=CARTESIAN_POINT('Ctrl Pts',(263.886426970624,81.772980327589,228.073593133703));
#19761=CARTESIAN_POINT('Ctrl Pts',(264.001135944375,82.2704599862669,228.073593133703));
#19762=CARTESIAN_POINT('Ctrl Pts',(264.146335943853,82.7685441967117,228.094687286035));
#19763=CARTESIAN_POINT('Ctrl Pts',(264.487097581211,83.7300632379758,228.176938403303));
#19764=CARTESIAN_POINT('Ctrl Pts',(264.682739293133,84.1958745673196,228.237768468517));
#19765=CARTESIAN_POINT('Ctrl Pts',(265.122345133427,85.0991343182584,228.395675688844));
#19766=CARTESIAN_POINT('Ctrl Pts',(265.366315246832,85.5365782245936,228.492763582321));
#19767=CARTESIAN_POINT('Ctrl Pts',(265.902443031719,86.3835668852031,228.720687561053));
#19768=CARTESIAN_POINT('Ctrl Pts',(266.192653439003,86.7895749064117,228.850739559984));
#19769=CARTESIAN_POINT('Ctrl Pts',(266.807294497184,87.5577921493384,229.134683190109));
#19770=CARTESIAN_POINT('Ctrl Pts',(267.132911069831,87.9218946153554,229.289088480638));
#19771=CARTESIAN_POINT('Ctrl Pts',(267.820387108045,88.6120665546024,229.618387505555));
#19772=CARTESIAN_POINT('Ctrl Pts',(268.180775004094,88.9363519636559,229.792575966063));
#19773=CARTESIAN_POINT('Ctrl Pts',(269.297122750516,89.8390387465664,230.329375212186));
#19774=CARTESIAN_POINT('Ctrl Pts',(270.092871176763,90.3537650523302,230.709036602005));
#19775=CARTESIAN_POINT('Ctrl Pts',(270.946701599761,90.7857513677001,231.090039190109));
#19776=CARTESIAN_POINT('',(274.135356630693,91.9232791773928,234.607407821084));
#19777=CARTESIAN_POINT('Ctrl Pts',(274.135356630693,91.9232791773928,234.607407821084));
#19778=CARTESIAN_POINT('Ctrl Pts',(274.135356630693,91.9232791773928,234.535038320367));
#19779=CARTESIAN_POINT('Ctrl Pts',(274.131436756292,91.9224288106584,234.463064877428));
#19780=CARTESIAN_POINT('Ctrl Pts',(274.123796303849,91.920744045495,234.391656669208));
#19781=CARTESIAN_POINT('Ctrl Pts',(274.115830884442,91.9189876231853,234.317211296794));
#19782=CARTESIAN_POINT('Ctrl Pts',(274.103821772655,91.9163242964729,234.243380425369));
#19783=CARTESIAN_POINT('Ctrl Pts',(274.088051837444,91.9127833752737,234.170349753486));
#19784=CARTESIAN_POINT('Ctrl Pts',(274.073492261134,91.9095142234529,234.102924261494));
#19785=CARTESIAN_POINT('Ctrl Pts',(274.055727958994,91.9054971820186,234.036180864883));
#19786=CARTESIAN_POINT('Ctrl Pts',(274.035019617716,91.9007632709779,233.970259652222));
#19787=CARTESIAN_POINT('Ctrl Pts',(274.030590092907,91.8997506849808,233.956159071058));
#19788=CARTESIAN_POINT('Ctrl Pts',(274.026022031944,91.8987044218231,233.942084342085));
#19789=CARTESIAN_POINT('Ctrl Pts',(274.021317425863,91.8976246431716,233.928036589951));
#19790=CARTESIAN_POINT('Ctrl Pts',(273.996549383788,91.8919400008002,233.854080277806));
#19791=CARTESIAN_POINT('Ctrl Pts',(273.968405853511,91.8854043574047,233.781795504628));
#19792=CARTESIAN_POINT('Ctrl Pts',(273.937311798586,91.8780563768258,233.711117184978));
#19793=CARTESIAN_POINT('Ctrl Pts',(273.905247128146,91.8704790255848,233.638232608412));
#19794=CARTESIAN_POINT('Ctrl Pts',(273.870044967459,91.8620378190554,233.567056334283));
#19795=CARTESIAN_POINT('Ctrl Pts',(273.832220155868,91.852783418526,233.497490874661));
#19796=CARTESIAN_POINT('Ctrl Pts',(273.811999181047,91.8478360574629,233.460301491602));
#19797=CARTESIAN_POINT('Ctrl Pts',(273.791029483462,91.842656431848,233.423572028953));
#19798=CARTESIAN_POINT('Ctrl Pts',(273.769394948025,91.8372532137308,233.387284706976));
#19799=CARTESIAN_POINT('Ctrl Pts',(273.75731872463,91.8342371809058,233.367029416177));
#19800=CARTESIAN_POINT('Ctrl Pts',(273.745028222076,91.8311496969879,233.346904585884));
#19801=CARTESIAN_POINT('Ctrl Pts',(273.732538525545,91.8279922984367,233.326908576382));
#19802=CARTESIAN_POINT('Ctrl Pts',(273.689569052797,91.8171296044821,233.258114432083));
#19803=CARTESIAN_POINT('Ctrl Pts',(273.64403282093,91.8053830652006,233.190632216215));
#19804=CARTESIAN_POINT('Ctrl Pts',(273.596418421607,91.792813601476,233.124621978395));
#19805=CARTESIAN_POINT('Ctrl Pts',(273.545891715675,91.7794753339275,233.054574263372));
#19806=CARTESIAN_POINT('Ctrl Pts',(273.493025268019,91.7652103828472,232.986184379854));
#19807=CARTESIAN_POINT('Ctrl Pts',(273.43845586753,91.750105172685,232.919622166538));
#19808=CARTESIAN_POINT('Ctrl Pts',(273.424728915839,91.7463054518098,232.902878418605));
#19809=CARTESIAN_POINT('Ctrl Pts',(273.410894432972,91.7424526253429,232.886250209042));
#19810=CARTESIAN_POINT('Ctrl Pts',(273.396962980695,91.7385481935867,232.869740012722));
#19811=CARTESIAN_POINT('Ctrl Pts',(273.379603236693,91.733682948068,232.849166939948));
#19812=CARTESIAN_POINT('Ctrl Pts',(273.36208638432,91.7287357448304,232.828771019452));
#19813=CARTESIAN_POINT('Ctrl Pts',(273.344430059197,91.723708600085,232.80855424713));
#19814=CARTESIAN_POINT('Ctrl Pts',(273.261137520052,91.6999933791896,232.713182968666));
#19815=CARTESIAN_POINT('Ctrl Pts',(273.174290846884,91.6743883805731,232.62123981037));
#19816=CARTESIAN_POINT('Ctrl Pts',(273.084583825663,91.6468908813567,232.532417612095));
#19817=CARTESIAN_POINT('Ctrl Pts',(273.043592822645,91.6343260892366,232.491830922805));
#19818=CARTESIAN_POINT('Ctrl Pts',(273.002005218492,91.6213661190327,232.451895635956));
#19819=CARTESIAN_POINT('Ctrl Pts',(272.959890653297,91.6080105790183,232.412581106915));
#19820=CARTESIAN_POINT('Ctrl Pts',(272.940882337097,91.6019825854623,232.394836580863));
#19821=CARTESIAN_POINT('Ctrl Pts',(272.921780141506,91.5958782675561,232.377232616759));
#19822=CARTESIAN_POINT('Ctrl Pts',(272.902591220157,91.5896979801168,232.359766120084));
#19823=CARTESIAN_POINT('Ctrl Pts',(272.770031813146,91.5470038013668,232.239105432614));
#19824=CARTESIAN_POINT('Ctrl Pts',(272.634389128362,91.5010339939522,232.125630805735));
#19825=CARTESIAN_POINT('Ctrl Pts',(272.496134800693,91.4515980170925,232.018444263631));
#19826=CARTESIAN_POINT('Ctrl Pts',(272.361709975531,91.4035313658842,231.914226678366));
#19827=CARTESIAN_POINT('Ctrl Pts',(272.224816181694,91.3521879483791,231.815953774217));
#19828=CARTESIAN_POINT('Ctrl Pts',(272.085906933541,91.2973816581163,231.722756196414));
#19829=CARTESIAN_POINT('Ctrl Pts',(272.053657844897,91.2846578622823,231.70111950204));
#19830=CARTESIAN_POINT('Ctrl Pts',(272.021300214268,91.271747374894,231.679756161252));
#19831=CARTESIAN_POINT('Ctrl Pts',(271.988839875611,91.2586477742405,231.658654931275));
#19832=CARTESIAN_POINT('Ctrl Pts',(271.975359761063,91.2532077780899,231.649892022169));
#19833=CARTESIAN_POINT('Ctrl Pts',(271.961862581456,91.2477354286293,231.641175220404));
#19834=CARTESIAN_POINT('Ctrl Pts',(271.948348777553,91.2422305660915,231.632503737925));
#19835=CARTESIAN_POINT('Ctrl Pts',(271.75944749256,91.1652814247133,231.511290333106));
#19836=CARTESIAN_POINT('Ctrl Pts',(271.567168706644,91.0819855798593,231.399173785266));
#19837=CARTESIAN_POINT('Ctrl Pts',(271.371685966445,90.991522850765,231.296407213572));
#19838=CARTESIAN_POINT('Ctrl Pts',(271.231645955151,90.9267171211585,231.222787251798));
#19839=CARTESIAN_POINT('Ctrl Pts',(271.089961938186,90.8582323944569,231.153965888954));
#19840=CARTESIAN_POINT('Ctrl Pts',(270.946701599761,90.7857513677001,231.090039190109));
#19841=CARTESIAN_POINT('',(274.135356630693,91.9232791773928,271.539778446323));
#19842=CARTESIAN_POINT('',(274.135356630693,91.9232791773928,225.073593133703));
#19843=CARTESIAN_POINT('',(270.946701599761,90.7857513677001,275.057147077298));
#19844=CARTESIAN_POINT('Ctrl Pts',(270.946701599761,90.7857513677001,275.057147077298));
#19845=CARTESIAN_POINT('Ctrl Pts',(271.147148719625,90.8871654312007,274.967702065628));
#19846=CARTESIAN_POINT('Ctrl Pts',(271.34476324736,90.9808826077627,274.868561523026));
#19847=CARTESIAN_POINT('Ctrl Pts',(271.539328407034,91.0677140898358,274.759933194106));
#19848=CARTESIAN_POINT('Ctrl Pts',(271.67685557422,91.1290903802882,274.683149938679));
#19849=CARTESIAN_POINT('Ctrl Pts',(271.81285958917,91.1870253136085,274.601626202326));
#19850=CARTESIAN_POINT('Ctrl Pts',(271.947269297188,91.2417907833522,274.515433600296));
#19851=CARTESIAN_POINT('Ctrl Pts',(271.961599095474,91.2476294846334,274.506244363752));
#19852=CARTESIAN_POINT('Ctrl Pts',(271.975910489673,91.2534319294108,274.497001196149));
#19853=CARTESIAN_POINT('Ctrl Pts',(271.990203132732,91.2591983338119,274.487703508352));
#19854=CARTESIAN_POINT('Ctrl Pts',(272.098285900434,91.3028046104674,274.417393221716));
#19855=CARTESIAN_POINT('Ctrl Pts',(272.205337551487,91.3443656947214,274.343942722402));
#19856=CARTESIAN_POINT('Ctrl Pts',(272.311082571951,91.3839252173294,274.267188431155));
#19857=CARTESIAN_POINT('Ctrl Pts',(272.35211269782,91.3992747078759,274.23740699826));
#19858=CARTESIAN_POINT('Ctrl Pts',(272.392946253339,91.4143230179486,274.207128671626));
#19859=CARTESIAN_POINT('Ctrl Pts',(272.433567745757,91.4290732808565,274.176345871292));
#19860=CARTESIAN_POINT('Ctrl Pts',(272.451959857466,91.435751727831,274.162408404479));
#19861=CARTESIAN_POINT('Ctrl Pts',(272.470318707282,91.4423720860675,274.14835848214));
#19862=CARTESIAN_POINT('Ctrl Pts',(272.488636890527,91.4489329051577,274.134198442038));
#19863=CARTESIAN_POINT('Ctrl Pts',(272.577176988614,91.4806443231537,274.06575653801));
#19864=CARTESIAN_POINT('Ctrl Pts',(272.664928571698,91.5110220617877,273.994616949445));
#19865=CARTESIAN_POINT('Ctrl Pts',(272.751028463175,91.539884748222,273.921056877197));
#19866=CARTESIAN_POINT('Ctrl Pts',(272.803061616885,91.5573274717141,273.876601971615));
#19867=CARTESIAN_POINT('Ctrl Pts',(272.854492132878,91.5742172229607,273.831263556676));
#19868=CARTESIAN_POINT('Ctrl Pts',(272.905137133368,91.590517678791,273.785106949247));
#19869=CARTESIAN_POINT('Ctrl Pts',(272.925013081086,91.596914894799,273.766992499505));
#19870=CARTESIAN_POINT('Ctrl Pts',(272.944773927187,91.6032238307619,273.748751578454));
#19871=CARTESIAN_POINT('Ctrl Pts',(272.964413382458,91.609444741243,273.730379919488));
#19872=CARTESIAN_POINT('Ctrl Pts',(273.034955955629,91.6317895072633,273.664391118936));
#19873=CARTESIAN_POINT('Ctrl Pts',(273.104021449973,91.6530265267405,273.596655216366));
#19874=CARTESIAN_POINT('Ctrl Pts',(273.171289389613,91.6731554332118,273.526995740641));
#19875=CARTESIAN_POINT('Ctrl Pts',(273.230376538101,91.6908363625213,273.465807902753));
#19876=CARTESIAN_POINT('Ctrl Pts',(273.288076906538,91.7076624974713,273.403136222412));
#19877=CARTESIAN_POINT('Ctrl Pts',(273.344191153207,91.7236405759986,273.338888375723));
#19878=CARTESIAN_POINT('Ctrl Pts',(273.36228644354,91.7287930637726,273.318170224663));
#19879=CARTESIAN_POINT('Ctrl Pts',(273.380235891361,91.7338618607828,273.297266495054));
#19880=CARTESIAN_POINT('Ctrl Pts',(273.398019690814,91.7388444962522,273.276177765194));
#19881=CARTESIAN_POINT('Ctrl Pts',(273.453966754319,91.7545196518199,273.209833533649));
#19882=CARTESIAN_POINT('Ctrl Pts',(273.508419834158,91.7693827426634,273.141518011198));
#19883=CARTESIAN_POINT('Ctrl Pts',(273.560758070633,91.7833496634919,273.071236177951));
#19884=CARTESIAN_POINT('Ctrl Pts',(273.610309195982,91.7965728190913,273.004696986654));
#19885=CARTESIAN_POINT('Ctrl Pts',(273.657964349937,91.8089927169614,272.936395433542));
#19886=CARTESIAN_POINT('Ctrl Pts',(273.70323469989,91.8205482289851,272.866362499145));
#19887=CARTESIAN_POINT('Ctrl Pts',(273.712961851203,91.8230311391919,272.851314659874));
#19888=CARTESIAN_POINT('Ctrl Pts',(273.722579057508,91.8254741813287,272.836186985488));
#19889=CARTESIAN_POINT('Ctrl Pts',(273.732081738571,91.8278768144873,272.820979949206));
#19890=CARTESIAN_POINT('Ctrl Pts',(273.744956668504,91.8311320782775,272.800376340041));
#19891=CARTESIAN_POINT('Ctrl Pts',(273.757607589668,91.8343101457514,272.779659819711));
#19892=CARTESIAN_POINT('Ctrl Pts',(273.770020895007,91.8374100213599,272.758824248661));
#19893=CARTESIAN_POINT('Ctrl Pts',(273.832725777213,91.8530688108257,272.653574922014));
#19894=CARTESIAN_POINT('Ctrl Pts',(273.88937815834,91.8667377350326,272.545434259877));
#19895=CARTESIAN_POINT('Ctrl Pts',(273.938616077441,91.8783669180643,272.433109113283));
#19896=CARTESIAN_POINT('Ctrl Pts',(273.969165785573,91.8855822544134,272.363416882029));
#19897=CARTESIAN_POINT('Ctrl Pts',(273.996862422025,91.8920119710173,272.292114942464));
#19898=CARTESIAN_POINT('Ctrl Pts',(274.021380084588,91.8976390244009,272.218897869882));
#19899=CARTESIAN_POINT('Ctrl Pts',(274.026196873887,91.8987445266264,272.204513496541));
#19900=CARTESIAN_POINT('Ctrl Pts',(274.030872599235,91.8998153772765,272.190089704733));
#19901=CARTESIAN_POINT('Ctrl Pts',(274.035405043613,91.9008513765542,272.175627657681));
#19902=CARTESIAN_POINT('Ctrl Pts',(274.055251319512,91.9053877206955,272.112302495372));
#19903=CARTESIAN_POINT('Ctrl Pts',(274.072276528136,91.9092391436709,272.048499558861));
#19904=CARTESIAN_POINT('Ctrl Pts',(274.08637809056,91.9124075875364,271.984215131047));
#19905=CARTESIAN_POINT('Ctrl Pts',(274.100128678601,91.9154971718687,271.921530681072));
#19906=CARTESIAN_POINT('Ctrl Pts',(274.111099813145,91.9179373759246,271.858387904451));
#19907=CARTESIAN_POINT('Ctrl Pts',(274.119153279711,91.9197187509681,271.794763406625));
#19908=CARTESIAN_POINT('Ctrl Pts',(274.126895998593,91.9214313906211,271.733593896994));
#19909=CARTESIAN_POINT('Ctrl Pts',(274.131942127975,91.922535058773,271.6719787108));
#19910=CARTESIAN_POINT('Ctrl Pts',(274.134123443669,91.923010727664,271.609884997458));
#19911=CARTESIAN_POINT('Ctrl Pts',(274.134941983491,91.9231892226569,271.586584299993));
#19912=CARTESIAN_POINT('Ctrl Pts',(274.135356629434,91.9232791771153,271.563216125089));
#19913=CARTESIAN_POINT('Ctrl Pts',(274.135356630693,91.9232791773928,271.539778446323));
#19914=CARTESIAN_POINT('Ctrl Pts',(270.946701599761,90.7857513677001,275.057147077298));
#19915=CARTESIAN_POINT('Ctrl Pts',(270.092103000801,90.3533764019677,275.438492446616));
#19916=CARTESIAN_POINT('Ctrl Pts',(269.294515045443,89.8375330431696,275.819048322909));
#19917=CARTESIAN_POINT('Ctrl Pts',(268.174370042181,88.9308682907682,276.357698561063));
#19918=CARTESIAN_POINT('Ctrl Pts',(267.812566862767,88.6046709104441,276.532563521238));
#19919=CARTESIAN_POINT('Ctrl Pts',(267.128003174131,87.9165036644382,276.860429416162));
#19920=CARTESIAN_POINT('Ctrl Pts',(266.803853181977,87.5536763209671,277.014109934142));
#19921=CARTESIAN_POINT('Ctrl Pts',(266.192094255626,86.7886894429728,277.296687835193));
#19922=CARTESIAN_POINT('Ctrl Pts',(265.904476993744,86.3865438599545,277.425604060267));
#19923=CARTESIAN_POINT('Ctrl Pts',(265.502051757571,85.7511352760914,277.596731851499));
#19924=CARTESIAN_POINT('Ctrl Pts',(265.372514445692,85.533418720424,277.650143627071));
#19925=CARTESIAN_POINT('Ctrl Pts',(265.12700712324,85.0930287132427,277.747519903133));
#19926=CARTESIAN_POINT('Ctrl Pts',(265.010589450995,84.8697087087132,277.791682801321));
#19927=CARTESIAN_POINT('Ctrl Pts',(264.68025597584,84.1903680227695,277.910250222304));
#19928=CARTESIAN_POINT('Ctrl Pts',(264.485195531666,83.7249952768337,277.970754033365));
#19929=CARTESIAN_POINT('Ctrl Pts',(264.146458099391,82.7685882982612,278.052422184988));
#19930=CARTESIAN_POINT('Ctrl Pts',(264.002516023709,82.2764452320033,278.073593133703));
#19931=CARTESIAN_POINT('Ctrl Pts',(263.886426970625,81.7729803275927,278.073593133703));
#19932=CARTESIAN_POINT('Origin',(292.894242939747,87.3992238969307,278.073593133703));
#19933=CARTESIAN_POINT('',(243.683501728549,98.7462478875858,234.607407821084));
#19934=CARTESIAN_POINT('',(243.683501728549,98.7462478875858,271.539778446323));
#19935=CARTESIAN_POINT('',(243.683501728549,98.7462478875858,278.073593133703));
#19936=CARTESIAN_POINT('',(273.255484225105,91.9275333837837,271.539778446323));
#19937=CARTESIAN_POINT('',(273.710942204595,91.8225137784534,271.539778446323));
#19938=CARTESIAN_POINT('',(273.255484225105,91.9275333837837,234.607407821084));
#19939=CARTESIAN_POINT('',(273.255484225105,91.9275333837837,233.452176263355));
#19940=CARTESIAN_POINT('',(243.683501728549,98.7462478875858,234.607407821084));
#19941=CARTESIAN_POINT('Origin',(257.611187373776,70.1353745599898,281.073593133703));
#19942=CARTESIAN_POINT('',(259.352493380025,77.6872189302482,273.85820282453));
#19943=CARTESIAN_POINT('',(259.352493380025,77.6872189302482,232.288983442877));
#19944=CARTESIAN_POINT('',(259.352493380025,77.6872189302482,281.073593133703));
#19945=CARTESIAN_POINT('Ctrl Pts',(259.352493380025,77.6872189302482,232.288983442877));
#19946=CARTESIAN_POINT('Ctrl Pts',(259.799729931322,77.5840950237155,232.288983442877));
#19947=CARTESIAN_POINT('Ctrl Pts',(260.231148369232,77.4433515176037,232.295963080489));
#19948=CARTESIAN_POINT('Ctrl Pts',(260.647156973428,77.2660829175506,232.311173103591));
#19949=CARTESIAN_POINT('Ctrl Pts',(260.786178632926,77.2068433376293,232.316255985606));
#19950=CARTESIAN_POINT('Ctrl Pts',(260.92347921877,77.1435243769817,232.322258048075));
#19951=CARTESIAN_POINT('Ctrl Pts',(261.059073483003,77.0761656990271,232.329226123689));
#19952=CARTESIAN_POINT('Ctrl Pts',(261.060375152847,77.0755190731517,232.329293015412));
#19953=CARTESIAN_POINT('Ctrl Pts',(261.061676665124,77.07487207515,232.329359996202));
#19954=CARTESIAN_POINT('Ctrl Pts',(261.062978019842,77.0742247050601,232.3294270661));
#19955=CARTESIAN_POINT('Ctrl Pts',(261.33228449996,76.9402558817594,232.343306723991));
#19956=CARTESIAN_POINT('Ctrl Pts',(261.596147266426,76.789265470937,232.361264709447));
#19957=CARTESIAN_POINT('Ctrl Pts',(261.849676263299,76.623649486148,232.384109654213));
#19958=CARTESIAN_POINT('Ctrl Pts',(261.851636577294,76.622368925199,232.38428629383));
#19959=CARTESIAN_POINT('Ctrl Pts',(261.8535962632,76.6210874966772,232.384463224748));
#19960=CARTESIAN_POINT('Ctrl Pts',(261.855555318817,76.619805201697,232.384640447333));
#19961=CARTESIAN_POINT('Ctrl Pts',(262.108186840548,76.4544458676261,232.407494321975));
#19962=CARTESIAN_POINT('Ctrl Pts',(262.348506811958,76.2761308640001,232.434981980953));
#19963=CARTESIAN_POINT('Ctrl Pts',(262.576984544395,76.0854467300596,232.468251468614));
#19964=CARTESIAN_POINT('Ctrl Pts',(262.579684340403,76.0831935202688,232.468644595896));
#19965=CARTESIAN_POINT('Ctrl Pts',(262.582382478871,76.0809385862697,232.469038530122));
#19966=CARTESIAN_POINT('Ctrl Pts',(262.58507896041,76.0786819291588,232.469433273148));
#19967=CARTESIAN_POINT('Ctrl Pts',(262.812349292638,75.8884817723865,232.502703806442));
#19968=CARTESIAN_POINT('Ctrl Pts',(263.027844148003,75.6860350266864,232.541716928009));
#19969=CARTESIAN_POINT('Ctrl Pts',(263.231485141018,75.4715486344357,232.588031737839));
#19970=CARTESIAN_POINT('Ctrl Pts',(263.23511017773,75.4677305375262,232.588856193089));
#19971=CARTESIAN_POINT('Ctrl Pts',(263.238731445518,75.4639086400978,232.589682957477));
#19972=CARTESIAN_POINT('Ctrl Pts',(263.242348944987,75.460082942514,232.590512039929));
#19973=CARTESIAN_POINT('Ctrl Pts',(263.403005120879,75.2901805142746,232.627332284797));
#19974=CARTESIAN_POINT('Ctrl Pts',(263.55696374067,75.1117051982107,232.669024678028));
#19975=CARTESIAN_POINT('Ctrl Pts',(263.701646453658,74.9279097715543,232.715699089282));
#19976=CARTESIAN_POINT('Ctrl Pts',(263.738889682465,74.8805984170229,232.727713695187));
#19977=CARTESIAN_POINT('Ctrl Pts',(263.775518302732,74.8329342760175,232.740058480346));
#19978=CARTESIAN_POINT('Ctrl Pts',(263.811488351603,74.7849723248566,232.752735451858));
#19979=CARTESIAN_POINT('Ctrl Pts',(263.816088319008,74.7788387937955,232.754356624405));
#19980=CARTESIAN_POINT('Ctrl Pts',(263.820677519938,74.7727003868462,232.755983225899));
#19981=CARTESIAN_POINT('Ctrl Pts',(263.82525585932,74.7665572228774,232.757615259359));
#19982=CARTESIAN_POINT('Ctrl Pts',(263.987229223509,74.5492231958706,232.815353650487));
#19983=CARTESIAN_POINT('Ctrl Pts',(264.136085850256,74.3259353125209,232.879765865605));
#19984=CARTESIAN_POINT('Ctrl Pts',(264.272124827383,74.09724671866,232.952014823533));
#19985=CARTESIAN_POINT('Ctrl Pts',(264.405225297936,73.8734979071372,233.022703169626));
#19986=CARTESIAN_POINT('Ctrl Pts',(264.526056135609,73.6445794265254,233.10089378503));
#19987=CARTESIAN_POINT('Ctrl Pts',(264.634929493928,73.4110199756965,233.187638901472));
#19988=CARTESIAN_POINT('Ctrl Pts',(264.656225433704,73.3653350801831,233.20460649395));
#19989=CARTESIAN_POINT('Ctrl Pts',(264.67706396797,73.3194726457758,233.221901259064));
#19990=CARTESIAN_POINT('Ctrl Pts',(264.697447567359,73.2734366659659,233.239530880404));
#19991=CARTESIAN_POINT('Ctrl Pts',(264.697447567358,73.2734366659668,272.907655386999));
#19992=CARTESIAN_POINT('Ctrl Pts',(264.593340011719,73.5085616425729,272.997697226476));
#19993=CARTESIAN_POINT('Ctrl Pts',(264.477362758326,73.739158912752,273.079000675102));
#19994=CARTESIAN_POINT('Ctrl Pts',(264.349198619934,73.9646996202116,273.152606789554));
#19995=CARTESIAN_POINT('Ctrl Pts',(264.218208011609,74.1952142933692,273.227836177661));
#19996=CARTESIAN_POINT('Ctrl Pts',(264.074486792083,74.420446661668,273.295025414564));
#19997=CARTESIAN_POINT('Ctrl Pts',(263.917729942372,74.6398427726569,273.355326969753));
#19998=CARTESIAN_POINT('Ctrl Pts',(263.887394022256,74.6823007763035,273.366996655412));
#19999=CARTESIAN_POINT('Ctrl Pts',(263.856570013268,74.7245402454938,273.378408500692));
#20000=CARTESIAN_POINT('Ctrl Pts',(263.82525585932,74.7665572228779,273.389571008044));
#20001=CARTESIAN_POINT('Ctrl Pts',(263.820677519938,74.7727003868467,273.391203041504));
#20002=CARTESIAN_POINT('Ctrl Pts',(263.816088319007,74.778838793796,273.392829642998));
#20003=CARTESIAN_POINT('Ctrl Pts',(263.811488351602,74.7849723248571,273.394450815546));
#20004=CARTESIAN_POINT('Ctrl Pts',(263.671751693772,74.9712951953743,273.443698389183));
#20005=CARTESIAN_POINT('Ctrl Pts',(263.522076037587,75.1531271579415,273.487933669545));
#20006=CARTESIAN_POINT('Ctrl Pts',(263.365038680784,75.3272284309448,273.527269693373));
#20007=CARTESIAN_POINT('Ctrl Pts',(263.324615206953,75.3720443804524,273.537395301459));
#20008=CARTESIAN_POINT('Ctrl Pts',(263.283703950786,75.4163478301469,273.547196213751));
#20009=CARTESIAN_POINT('Ctrl Pts',(263.242348944987,75.4600829425142,273.556674227475));
#20010=CARTESIAN_POINT('Ctrl Pts',(263.238731445518,75.4639086400981,273.557503309927));
#20011=CARTESIAN_POINT('Ctrl Pts',(263.23511017773,75.4677305375265,273.558330074314));
#20012=CARTESIAN_POINT('Ctrl Pts',(263.231485141018,75.471548634436,273.559154529565));
#20013=CARTESIAN_POINT('Ctrl Pts',(263.027844148002,75.6860350266869,273.605469339391));
#20014=CARTESIAN_POINT('Ctrl Pts',(262.812349292638,75.8884817723866,273.644482460965));
#20015=CARTESIAN_POINT('Ctrl Pts',(262.58507896041,76.0786819291588,273.677752994258));
#20016=CARTESIAN_POINT('Ctrl Pts',(262.582382478871,76.0809385862696,273.678147737285));
#20017=CARTESIAN_POINT('Ctrl Pts',(262.579684340403,76.0831935202688,273.678541671511));
#20018=CARTESIAN_POINT('Ctrl Pts',(262.576984544395,76.0854467300596,273.678934798793));
#20019=CARTESIAN_POINT('Ctrl Pts',(262.348506811958,76.2761308640001,273.712204286454));
#20020=CARTESIAN_POINT('Ctrl Pts',(262.108186840548,76.4544458676262,273.739691945435));
#20021=CARTESIAN_POINT('Ctrl Pts',(261.855555318817,76.6198052016969,273.762545820075));
#20022=CARTESIAN_POINT('Ctrl Pts',(261.853596263201,76.6210874966771,273.762723042661));
#20023=CARTESIAN_POINT('Ctrl Pts',(261.851636577294,76.6223689251989,273.762899973578));
#20024=CARTESIAN_POINT('Ctrl Pts',(261.849676263299,76.6236494861479,273.763076613196));
#20025=CARTESIAN_POINT('Ctrl Pts',(261.596147266426,76.789265470937,273.785921557959));
#20026=CARTESIAN_POINT('Ctrl Pts',(261.33228449996,76.9402558817594,273.803879543416));
#20027=CARTESIAN_POINT('Ctrl Pts',(261.062978019842,77.0742247050601,273.817759201306));
#20028=CARTESIAN_POINT('Ctrl Pts',(261.061676665124,77.07487207515,273.817826271204));
#20029=CARTESIAN_POINT('Ctrl Pts',(261.060375152847,77.0755190731518,273.817893251995));
#20030=CARTESIAN_POINT('Ctrl Pts',(261.059073483003,77.0761656990271,273.817960143717));
#20031=CARTESIAN_POINT('Ctrl Pts',(260.65332096387,77.2777299275741,273.838811425665));
#20032=CARTESIAN_POINT('Ctrl Pts',(260.23229067611,77.4431241300129,273.85101306254));
#20033=CARTESIAN_POINT('Ctrl Pts',(259.795580893516,77.5712698272539,273.855817711116));
#20034=CARTESIAN_POINT('Ctrl Pts',(259.649641401155,77.614093502722,273.857423326566));
#20035=CARTESIAN_POINT('Ctrl Pts',(259.501950724621,77.6527570214662,273.85820282453));
#20036=CARTESIAN_POINT('Ctrl Pts',(259.352493380025,77.6872189302482,273.85820282453));
#20037=CARTESIAN_POINT('Origin',(239.8638627471,82.1809118495999,281.073593133703));
#20038=CARTESIAN_POINT('',(239.8638627471,82.1809118495999,273.85820282453));
#20039=CARTESIAN_POINT('',(239.8638627471,82.1809118495999,232.288983442877));
#20040=CARTESIAN_POINT('',(239.8638627471,82.1809118495999,281.073593133703));
#20041=CARTESIAN_POINT('',(259.352493380025,77.6872189302482,232.288983442877));
#20042=CARTESIAN_POINT('',(239.8638627471,82.1809118495999,273.85820282453));
#20043=CARTESIAN_POINT('Origin',(277.041252647849,78.7397376070303,225.073593133703));
#20044=CARTESIAN_POINT('Origin',(277.041252647849,78.7397376070303,281.073593133703));
#20045=CARTESIAN_POINT('Origin',(240.987285976938,87.0530695078311,253.073593133703));
#20046=CARTESIAN_POINT('Origin',(240.313232039036,84.1297749128924,232.288983442877));
#20047=CARTESIAN_POINT('Origin',(240.313232039036,84.1297749128924,273.85820282453));
#20048=CARTESIAN_POINT('Origin',(240.987285976938,87.0530695078311,253.073593133703));
#20049=CARTESIAN_POINT('Origin',(243.234132436614,96.7973848242934,234.607407821084));
#20050=CARTESIAN_POINT('Origin',(243.234132436614,96.7973848242934,271.539778446323));
#20051=CARTESIAN_POINT('Origin',(221.231335829438,119.31686398042,253.073593133703));
#20052=CARTESIAN_POINT('Origin',(142.827444005805,135.342772594535,253.073593133703));
#20053=CARTESIAN_POINT('Origin',(141.515985505207,134.105809943033,253.073593133703));
#20054=CARTESIAN_POINT('Origin',(136.531485523992,134.742017407048,253.073593133703));
#20055=CARTESIAN_POINT('',(133.779098610889,122.805231144382,271.693139315069));
#20056=CARTESIAN_POINT('',(136.194458555041,133.280370109579,253.073593133703));
#20057=CARTESIAN_POINT('',(133.779098610889,122.805231144382,271.693139315069));
#20058=CARTESIAN_POINT('',(128.948378722586,101.854953213988,271.693139315069));
#20059=CARTESIAN_POINT('',(128.948378722586,101.854953213988,271.693139315069));
#20060=CARTESIAN_POINT('',(126.533018778434,91.3798142487909,253.073593133703));
#20061=CARTESIAN_POINT('',(126.533018778434,91.3798142487909,253.073593133703));
#20062=CARTESIAN_POINT('',(128.948378722586,101.854953213988,234.454046952338));
#20063=CARTESIAN_POINT('',(128.948378722586,101.854953213988,234.454046952338));
#20064=CARTESIAN_POINT('',(133.779098610889,122.805231144382,234.454046952338));
#20065=CARTESIAN_POINT('',(133.779098610889,122.805231144382,234.454046952338));
#20066=CARTESIAN_POINT('',(136.194458555041,133.280370109579,253.073593133703));
#20067=CARTESIAN_POINT('Origin',(127.445293655188,124.265681343171,271.693139315069));
#20068=CARTESIAN_POINT('',(130.835085130986,134.516135662401,253.073593133703));
#20069=CARTESIAN_POINT('',(129.86065359934,134.740820308368,253.073593133703));
#20070=CARTESIAN_POINT('',(128.419725186835,124.040996697204,271.693139315069));
#20071=CARTESIAN_POINT('',(128.419725186835,124.040996697204,271.693139315069));
#20072=CARTESIAN_POINT('',(127.445293655188,124.265681343171,271.693139315069));
#20073=CARTESIAN_POINT('Origin',(129.86065359934,134.740820308368,253.073593133703));
#20074=CARTESIAN_POINT('',(128.419725186835,124.040996697204,234.454046952338));
#20075=CARTESIAN_POINT('',(127.445293655188,124.265681343171,234.454046952338));
#20076=CARTESIAN_POINT('',(130.835085130986,134.516135662401,253.073593133703));
#20077=CARTESIAN_POINT('Origin',(127.445293655188,124.265681343171,234.454046952338));
#20078=CARTESIAN_POINT('',(123.589005298532,103.09071876681,234.454046952338));
#20079=CARTESIAN_POINT('',(122.614573766885,103.315403412777,234.454046952338));
#20080=CARTESIAN_POINT('',(128.419725186835,124.040996697204,234.454046952338));
#20081=CARTESIAN_POINT('Origin',(122.614573766885,103.315403412777,234.454046952338));
#20082=CARTESIAN_POINT('',(121.17364535438,92.6155798016126,253.073593133703));
#20083=CARTESIAN_POINT('',(120.199213822734,92.8402644475802,253.073593133703));
#20084=CARTESIAN_POINT('',(123.589005298532,103.09071876681,234.454046952338));
#20085=CARTESIAN_POINT('Origin',(120.199213822734,92.8402644475802,253.073593133703));
#20086=CARTESIAN_POINT('',(123.589005298532,103.09071876681,271.693139315069));
#20087=CARTESIAN_POINT('',(122.614573766885,103.315403412777,271.693139315069));
#20088=CARTESIAN_POINT('',(121.17364535438,92.6155798016126,253.073593133703));
#20089=CARTESIAN_POINT('Origin',(122.614573766885,103.315403412777,271.693139315069));
#20090=CARTESIAN_POINT('',(123.589005298532,103.09071876681,271.693139315069));
#20091=CARTESIAN_POINT('Origin',(125.029933711037,113.790542377974,253.073593133703));
#20092=CARTESIAN_POINT('',(120.458657304398,93.9654410617858,253.073593133703));
#20093=CARTESIAN_POINT('',(122.744295507717,103.87799171988,270.693139315069));
#20094=CARTESIAN_POINT('',(122.809156378134,104.159285873431,271.193139315069));
#20095=CARTESIAN_POINT('',(127.315571914356,123.703093036068,270.693139315069));
#20096=CARTESIAN_POINT('',(127.445293655188,124.265681343171,270.693139315069));
#20097=CARTESIAN_POINT('',(129.601210117676,133.615643694162,253.073593133703));
#20098=CARTESIAN_POINT('',(129.666070988092,133.896937847714,252.573593133703));
#20099=CARTESIAN_POINT('',(127.315571914356,123.703093036068,235.454046952338));
#20100=CARTESIAN_POINT('',(127.25071104394,123.421798882517,234.954046952338));
#20101=CARTESIAN_POINT('',(122.744295507717,103.87799171988,235.454046952338));
#20102=CARTESIAN_POINT('',(122.614573766885,103.315403412777,235.454046952338));
#20103=CARTESIAN_POINT('',(120.393796433982,93.6841469082344,253.573593133703));
#20104=CARTESIAN_POINT('Origin',(257.838634424508,160.135434381298,253.073593133703));
#20105=CARTESIAN_POINT('',(237.375572259937,164.853811946618,253.073593133703));
#20106=CARTESIAN_POINT('',(233.477846133352,165.752550530488,253.073593133703));
#20107=CARTESIAN_POINT('',(233.477846133352,165.752550530488,253.073593133703));
#20108=CARTESIAN_POINT('',(237.375572259937,164.853811946618,265.706741519111));
#20109=CARTESIAN_POINT('',(237.375572259937,164.853811946618,265.706741519111));
#20110=CARTESIAN_POINT('',(233.477846133352,165.752550530488,265.706741519111));
#20111=CARTESIAN_POINT('',(233.477846133352,165.752550530488,265.706741519111));
#20112=CARTESIAN_POINT('',(233.477846133352,165.752550530488,269.073593133703));
#20113=CARTESIAN_POINT('',(233.477846133352,165.752550530488,265.706741519111));
#20114=CARTESIAN_POINT('',(233.477846133352,165.752550530488,269.073593133703));
#20115=CARTESIAN_POINT('',(233.477846133352,165.752550530488,251.073593133703));
#20116=CARTESIAN_POINT('',(246.891390975948,162.65965228546,251.073593133703));
#20117=CARTESIAN_POINT('',(233.477846133352,165.752550530488,251.073593133703));
#20118=CARTESIAN_POINT('Origin',(216.626497685783,92.6701856570208,253.073593133703));
#20119=CARTESIAN_POINT('',(219.996767375296,107.286658631714,269.073593133703));
#20120=CARTESIAN_POINT('',(234.488927040206,170.137492422896,265.706741519111));
#20121=CARTESIAN_POINT('',(234.488927040206,170.137492422896,265.706741519111));
#20122=CARTESIAN_POINT('',(234.488927040206,170.137492422896,253.073593133703));
#20123=CARTESIAN_POINT('',(234.488927040206,170.137492422896,265.706741519111));
#20124=CARTESIAN_POINT('',(234.488927040206,170.137492422896,253.073593133703));
#20125=CARTESIAN_POINT('',(219.996767375296,107.286658631714,251.073593133703));
#20126=CARTESIAN_POINT('Origin',(240.987285976938,87.0530695078311,251.073593133703));
#20127=CARTESIAN_POINT('',(237.536534944929,103.242335004298,251.073593133703));
#20128=CARTESIAN_POINT('Origin',(240.987285976938,87.0530695078311,269.073593133703));
#20129=CARTESIAN_POINT('',(237.536534944929,103.242335004298,269.073593133703));
#20130=CARTESIAN_POINT('Origin',(232.801789355145,89.9740347659234,253.073593133703));
#20131=CARTESIAN_POINT('Origin',(234.488927040206,170.137492422896,265.706741519111));
#20132=CARTESIAN_POINT('',(237.712599228888,166.315459244087,265.706741519111));
#20133=CARTESIAN_POINT('',(238.386653166791,169.238753839026,265.706741519111));
#20134=CARTESIAN_POINT('',(235.463358571852,169.912807776929,265.706741519111));
#20135=CARTESIAN_POINT('Origin',(234.789304633949,166.98951318199,265.706741519111));
#20136=CARTESIAN_POINT('',(234.488927040206,170.137492422896,265.706741519111));
#20137=CARTESIAN_POINT('Origin',(238.386653166791,169.238753839026,265.706741519111));
#20138=CARTESIAN_POINT('',(237.712599228888,166.315459244087,253.073593133703));
#20139=CARTESIAN_POINT('',(238.386653166791,169.238753839026,253.073593133703));
#20140=CARTESIAN_POINT('',(237.712599228888,166.315459244087,265.706741519111));
#20141=CARTESIAN_POINT('Origin',(234.488927040206,170.137492422896,253.073593133703));
#20142=CARTESIAN_POINT('',(235.463358571852,169.912807776929,253.073593133703));
#20143=CARTESIAN_POINT('',(234.488927040206,170.137492422896,253.073593133703));
#20144=CARTESIAN_POINT('Origin',(234.789304633949,166.98951318199,253.073593133703));
#20145=CARTESIAN_POINT('Origin',(258.849715331362,164.520376273706,253.073593133703));
#20146=CARTESIAN_POINT('',(235.463358571852,169.912807776929,253.073593133703));
#20147=CARTESIAN_POINT('Origin',(245.930348188225,108.490563204048,253.073593133703));
#20148=CARTESIAN_POINT('',(267.855057650266,103.435158669777,256.243466114781));
#20149=CARTESIAN_POINT('',(267.855057650266,103.435158669777,264.903720152625));
#20150=CARTESIAN_POINT('',(267.855057650266,103.435158669777,256.243466114781));
#20151=CARTESIAN_POINT('Origin',(245.930348188225,108.490563204048,253.073593133703));
#20152=CARTESIAN_POINT('',(260.546821162919,105.120293514534,251.913339095859));
#20153=CARTESIAN_POINT('',(267.855057650266,103.435158669777,256.243466114781));
#20154=CARTESIAN_POINT('',(260.546821162919,105.120293514534,251.913339095859));
#20155=CARTESIAN_POINT('Origin',(245.930348188225,108.490563204048,253.073593133703));
#20156=CARTESIAN_POINT('',(253.238584675572,106.805428359291,256.243466114781));
#20157=CARTESIAN_POINT('',(260.546821162919,105.120293514534,251.913339095859));
#20158=CARTESIAN_POINT('',(253.238584675572,106.805428359291,256.243466114781));
#20159=CARTESIAN_POINT('Origin',(245.930348188225,108.490563204048,253.073593133703));
#20160=CARTESIAN_POINT('',(253.238584675572,106.805428359291,264.903720152625));
#20161=CARTESIAN_POINT('',(253.238584675572,106.805428359291,256.243466114781));
#20162=CARTESIAN_POINT('',(253.238584675572,106.805428359291,264.903720152625));
#20163=CARTESIAN_POINT('Origin',(245.930348188225,108.490563204048,253.073593133703));
#20164=CARTESIAN_POINT('',(260.546821162919,105.120293514534,269.233847171548));
#20165=CARTESIAN_POINT('',(253.238584675572,106.805428359291,264.903720152625));
#20166=CARTESIAN_POINT('',(260.546821162919,105.120293514534,269.233847171548));
#20167=CARTESIAN_POINT('Origin',(245.930348188225,108.490563204048,253.073593133703));
#20168=CARTESIAN_POINT('',(267.855057650266,103.435158669777,264.903720152625));
#20169=CARTESIAN_POINT('',(260.546821162919,105.120293514534,269.233847171548));
#20170=CARTESIAN_POINT('',(267.855057650266,103.435158669777,264.903720152625));
#20171=CARTESIAN_POINT('Origin',(256.608854365086,121.421901333985,264.903720152625));
#20172=CARTESIAN_POINT('',(259.941647761247,120.140305384201,266.944961604945));
#20173=CARTESIAN_POINT('',(256.496512042102,120.934685568162,264.903720152625));
#20174=CARTESIAN_POINT('',(256.291289789483,120.044660203559,264.903720152625));
#20175=CARTESIAN_POINT('Origin',(253.318991306379,107.15414269192,264.903720152651));
#20176=CARTESIAN_POINT('',(256.608854365086,121.421901333985,264.903720152625));
#20177=CARTESIAN_POINT('',(263.917090852433,119.736766489228,269.233847171548));
#20178=CARTESIAN_POINT('Origin',(263.917090852433,119.736766489228,269.233847171548));
#20179=CARTESIAN_POINT('',(267.66784929765,118.358796062609,266.944961604945));
#20180=CARTESIAN_POINT('',(263.804748529449,119.249550723405,269.233847171548));
#20181=CARTESIAN_POINT('',(270.907762764176,116.674390514045,264.903720152625));
#20182=CARTESIAN_POINT('',(271.225327339779,118.051631644471,264.903720152625));
#20183=CARTESIAN_POINT('Origin',(267.935464280873,103.783873001336,264.903720152574));
#20184=CARTESIAN_POINT('Origin',(271.225327339779,118.051631644471,264.903720152625));
#20185=CARTESIAN_POINT('',(271.112985016796,117.564415878648,260.32594901942));
#20186=CARTESIAN_POINT('',(271.112985016796,117.564415878648,260.821237247987));
#20187=CARTESIAN_POINT('',(271.112985016796,117.564415878648,264.903720152625));
#20188=CARTESIAN_POINT('Origin',(267.935464280956,103.783873002082,264.90372015265));
#20189=CARTESIAN_POINT('',(270.907762764176,116.674390514045,256.243466114781));
#20190=CARTESIAN_POINT('',(271.225327339779,118.051631644471,256.243466114781));
#20191=CARTESIAN_POINT('Origin',(267.935464280502,103.783873000137,256.243466114489));
#20192=CARTESIAN_POINT('Origin',(271.225327339779,118.051631644471,256.243466114781));
#20193=CARTESIAN_POINT('',(267.66784929765,118.358796062609,254.202224662462));
#20194=CARTESIAN_POINT('',(271.112985016796,117.564415878648,256.243466114781));
#20195=CARTESIAN_POINT('Origin',(267.935464280876,103.783873001347,256.243466114831));
#20196=CARTESIAN_POINT('',(263.917090852433,119.736766489228,251.913339095859));
#20197=CARTESIAN_POINT('Origin',(263.917090852433,119.736766489228,251.913339095859));
#20198=CARTESIAN_POINT('',(256.291289789483,120.044660203559,256.243466114781));
#20199=CARTESIAN_POINT('',(256.608854365086,121.421901333985,256.243466114781));
#20200=CARTESIAN_POINT('',(259.941647761247,120.140305384201,254.202224662462));
#20201=CARTESIAN_POINT('Origin',(253.318991306673,107.154142692754,256.243466114698));
#20202=CARTESIAN_POINT('',(263.804748529449,119.249550723405,251.913339095859));
#20203=CARTESIAN_POINT('Origin',(256.608854365086,121.421901333985,256.243466114781));
#20204=CARTESIAN_POINT('',(256.496512042102,120.934685568162,260.821237247987));
#20205=CARTESIAN_POINT('Origin',(253.318991306164,107.154142691181,264.903720152705));
#20206=CARTESIAN_POINT('',(256.496512042102,120.934685568162,260.32594901942));
#20207=CARTESIAN_POINT('',(256.496512042102,120.934685568162,256.243466114781));
#20208=CARTESIAN_POINT('Origin',(253.31899130647,107.15414269249,256.243466114903));
#20209=CARTESIAN_POINT('Origin',(249.300617877739,123.107036178742,253.073593133703));
#20210=CARTESIAN_POINT('',(257.096169703538,121.309536051521,260.573593133703));
#20211=CARTESIAN_POINT('Origin',(270.876613007385,118.132038275181,264.697107058593));
#20212=CARTESIAN_POINT('Origin',(270.876613007503,118.132038275155,256.450079208744));
#20213=CARTESIAN_POINT('',(270.738012001328,118.163996926934,260.573593133704));
#20214=CARTESIAN_POINT('Origin',(256.957568697313,121.341494703312,256.450079208715));
#20215=CARTESIAN_POINT('Origin',(256.957568697334,121.341494703307,264.69710705868));
#20216=CARTESIAN_POINT('Origin',(246.379666533197,123.780549809431,258.265580431811));
#20217=CARTESIAN_POINT('',(255.562088621698,117.401987874335,269.05363105279));
#20218=CARTESIAN_POINT('Origin',(259.529805709628,120.748387703296,271.255961488578));
#20219=CARTESIAN_POINT('',(265.586365399582,121.687840922005,265.342093607999));
#20220=CARTESIAN_POINT('Origin',(257.096070130909,121.309559011001,253.073593133703));
#20221=CARTESIAN_POINT('',(257.010851567994,121.256276140383,260.573593133703));
#20222=CARTESIAN_POINT('',(259.309178347426,122.693303992497,259.466995116294));
#20223=CARTESIAN_POINT('',(254.858613753559,119.910590352186,259.537334008256));
#20224=CARTESIAN_POINT('Origin',(270.738111573956,118.163973967455,253.073593133703));
#20225=CARTESIAN_POINT('',(270.791394444574,118.078755404539,260.573593133703));
#20226=CARTESIAN_POINT('',(272.137080232772,115.926517590104,259.537334008256));
#20227=CARTESIAN_POINT('',(269.35436659246,120.377082183972,259.466995116294));
#20228=CARTESIAN_POINT('Origin',(252.708784988104,122.321180225069,259.131605835595));
#20229=CARTESIAN_POINT('',(257.787370918632,118.793344694491,253.164983786045));
#20230=CARTESIAN_POINT('Origin',(253.200687254721,122.207757287658,246.141224778829));
#20231=CARTESIAN_POINT('',(264.195008579426,123.913123218939,256.876521230836));
#20232=CARTESIAN_POINT('Origin',(259.161112492359,117.81723196461,263.000245587794));
#20233=CARTESIAN_POINT('Origin',(262.430485695863,112.851978297123,260.573593240362));
#20234=CARTESIAN_POINT('Origin',(260.875334786248,115.075571113603,259.466995116294));
#20235=CARTESIAN_POINT('Origin',(259.643746269855,111.10869307224,259.288708143003));
#20236=CARTESIAN_POINT('Origin',(262.271656097715,112.843043970938,260.573593172734));
#20237=CARTESIAN_POINT('Origin',(264.610689417795,114.214272186285,259.466995116294));
#20238=CARTESIAN_POINT('Origin',(290.197052756605,75.7062702018219,253.073593133703));
#20239=CARTESIAN_POINT('',(261.613491303351,78.6976913251852,230.342590522438));
#20240=CARTESIAN_POINT('',(259.737667058827,79.3576729844988,230.309496805655));
#20241=CARTESIAN_POINT('Ctrl Pts',(261.613491303076,78.6976913253861,230.342590522417));
#20242=CARTESIAN_POINT('Ctrl Pts',(261.012965195301,78.9874393341337,230.31984533521));
#20243=CARTESIAN_POINT('Ctrl Pts',(260.387795558813,79.2077662059219,230.309496805655));
#20244=CARTESIAN_POINT('Ctrl Pts',(259.737667058827,79.3576729844988,230.309496805655));
#20245=CARTESIAN_POINT('',(289.458803205568,72.5045665978414,230.309496805655));
#20246=CARTESIAN_POINT('',(269.82981977108,91.6423159687713,232.848723505596));
#20247=CARTESIAN_POINT('',(292.657884593393,86.3786155484235,232.848723505596));
#20248=CARTESIAN_POINT('Ctrl Pts',(269.82981977108,91.6423159687712,232.848723505596));
#20249=CARTESIAN_POINT('Ctrl Pts',(269.412062867116,91.4518718255699,232.697399160319));
#20250=CARTESIAN_POINT('Ctrl Pts',(269.005494956222,91.2443405944999,232.545799518012));
#20251=CARTESIAN_POINT('Ctrl Pts',(268.609998824741,91.018971085966,232.395516517388));
#20252=CARTESIAN_POINT('Ctrl Pts',(268.222148036074,90.7979581994462,232.248138640147));
#20253=CARTESIAN_POINT('Ctrl Pts',(267.844945108691,90.5597901305427,232.102027006344));
#20254=CARTESIAN_POINT('Ctrl Pts',(267.478273206019,90.3037347924297,231.958726010898));
#20255=CARTESIAN_POINT('Ctrl Pts',(267.137265294114,90.0656012033941,231.82545489611));
#20256=CARTESIAN_POINT('Ctrl Pts',(266.805365789826,89.8119965611551,231.694615072261));
#20257=CARTESIAN_POINT('Ctrl Pts',(266.482475600845,89.5423115743041,231.567483405361));
#20258=CARTESIAN_POINT('Ctrl Pts',(266.463505779451,89.5264675622914,231.560014410957));
#20259=CARTESIAN_POINT('Ctrl Pts',(266.444566559758,89.5105672705819,231.552557898557));
#20260=CARTESIAN_POINT('Ctrl Pts',(266.425658042599,89.4946106679016,231.545114183402));
#20261=CARTESIAN_POINT('Ctrl Pts',(266.224546364397,89.3248956597622,231.465942557493));
#20262=CARTESIAN_POINT('Ctrl Pts',(266.026936720047,89.148522798973,231.388184363742));
#20263=CARTESIAN_POINT('Ctrl Pts',(265.83461601482,88.9669001566157,231.312816009738));
#20264=CARTESIAN_POINT('Ctrl Pts',(265.800972613982,88.9351282090711,231.299631533624));
#20265=CARTESIAN_POINT('Ctrl Pts',(265.767491061666,88.9031957372929,231.286520197391));
#20266=CARTESIAN_POINT('Ctrl Pts',(265.734180908561,88.8711104332793,231.273487229652));
#20267=CARTESIAN_POINT('Ctrl Pts',(265.714141013639,88.8518074262067,231.265646397963));
#20268=CARTESIAN_POINT('Ctrl Pts',(265.69416030416,88.8324465029543,231.257832863114));
#20269=CARTESIAN_POINT('Ctrl Pts',(265.674240936888,88.8130292915668,231.250047785851));
#20270=CARTESIAN_POINT('Ctrl Pts',(265.472975056506,88.6168372092048,231.17138713325));
#20271=CARTESIAN_POINT('Ctrl Pts',(265.277392278449,88.4144325332718,231.095401978004));
#20272=CARTESIAN_POINT('Ctrl Pts',(265.087752747776,88.2057836732551,231.022485409116));
#20273=CARTESIAN_POINT('Ctrl Pts',(265.069859489022,88.1860968071894,231.015605435146));
#20274=CARTESIAN_POINT('Ctrl Pts',(265.052019113926,88.1663543769224,231.008752771387));
#20275=CARTESIAN_POINT('Ctrl Pts',(265.03423182395,88.1465563722257,231.00192774245));
#20276=CARTESIAN_POINT('Ctrl Pts',(265.014562170462,88.1246632174707,230.994380445789));
#20277=CARTESIAN_POINT('Ctrl Pts',(264.994956786706,88.1027013973482,230.986866698014));
#20278=CARTESIAN_POINT('Ctrl Pts',(264.975415760474,88.0806706935066,230.979386876402));
#20279=CARTESIAN_POINT('Ctrl Pts',(264.771466620346,87.850736858316,230.901320189011));
#20280=CARTESIAN_POINT('Ctrl Pts',(264.574526846944,87.6133013235892,230.826946705393));
#20281=CARTESIAN_POINT('Ctrl Pts',(264.384829486875,87.3680005217492,230.756727452304));
#20282=CARTESIAN_POINT('Ctrl Pts',(264.366629531072,87.3444658571115,230.7499904724));
#20283=CARTESIAN_POINT('Ctrl Pts',(264.348495277114,87.3208574571962,230.743291364523));
#20284=CARTESIAN_POINT('Ctrl Pts',(264.330427274506,87.2971753749938,230.73663066703));
#20285=CARTESIAN_POINT('Ctrl Pts',(264.192051910297,87.1158040955474,230.685619137893));
#20286=CARTESIAN_POINT('Ctrl Pts',(264.057307830443,86.9296671023993,230.636776967807));
#20287=CARTESIAN_POINT('Ctrl Pts',(263.927380064349,86.7402318307243,230.590657569167));
#20288=CARTESIAN_POINT('Ctrl Pts',(263.880505355907,86.6718882934231,230.574018836509));
#20289=CARTESIAN_POINT('Ctrl Pts',(263.834257363913,86.6031159271292,230.5577343861));
#20290=CARTESIAN_POINT('Ctrl Pts',(263.788690979733,86.5339850002118,230.541829743817));
#20291=CARTESIAN_POINT('Ctrl Pts',(263.77298301991,86.5101537078662,230.536346985278));
#20292=CARTESIAN_POINT('Ctrl Pts',(263.75735496487,86.4862783657571,230.530909020002));
#20293=CARTESIAN_POINT('Ctrl Pts',(263.741808862961,86.4623615195282,230.525516828383));
#20294=CARTESIAN_POINT('Ctrl Pts',(263.484549544799,86.066581819303,230.436286000791));
#20295=CARTESIAN_POINT('Ctrl Pts',(263.248690603452,85.6584941433215,230.359194420258));
#20296=CARTESIAN_POINT('Ctrl Pts',(263.034697118873,85.2379084504163,230.295174158128));
#20297=CARTESIAN_POINT('Ctrl Pts',(262.951489163286,85.0743704075428,230.270280899633));
#20298=CARTESIAN_POINT('Ctrl Pts',(262.871586616947,84.9089430262691,230.247363811953));
#20299=CARTESIAN_POINT('Ctrl Pts',(262.79501499609,84.7416161629987,230.226477214704));
#20300=CARTESIAN_POINT('Ctrl Pts',(262.785462820506,84.7207424298838,230.223871648281));
#20301=CARTESIAN_POINT('Ctrl Pts',(262.775962440878,84.699838964399,230.221297659614));
#20302=CARTESIAN_POINT('Ctrl Pts',(262.766513896054,84.6789057298734,230.218755353273));
#20303=CARTESIAN_POINT('Ctrl Pts',(262.634811555875,84.3871194256535,230.183318394364));
#20304=CARTESIAN_POINT('Ctrl Pts',(262.513220219422,84.0895305978623,230.154044317955));
#20305=CARTESIAN_POINT('Ctrl Pts',(262.402090716589,83.7859199686843,230.131279947247));
#20306=CARTESIAN_POINT('Ctrl Pts',(262.395546655457,83.7680413094,230.129939426236));
#20307=CARTESIAN_POINT('Ctrl Pts',(262.389038572057,83.7501409057057,230.128621416215));
#20308=CARTESIAN_POINT('Ctrl Pts',(262.382566616886,83.7322188864832,230.127326007806));
#20309=CARTESIAN_POINT('Ctrl Pts',(262.312662251443,83.5386410034226,230.113334145927));
#20310=CARTESIAN_POINT('Ctrl Pts',(262.246832138757,83.3419473504265,230.101977077434));
#20311=CARTESIAN_POINT('Ctrl Pts',(262.185666534111,83.1437789606774,230.093387800197));
#20312=CARTESIAN_POINT('Ctrl Pts',(262.149430174372,83.0263779948678,230.088299251794));
#20313=CARTESIAN_POINT('Ctrl Pts',(262.114830284334,82.908460176112,230.084181676947));
#20314=CARTESIAN_POINT('Ctrl Pts',(262.081982731389,82.7903697894063,230.081058549722));
#20315=CARTESIAN_POINT('Ctrl Pts',(262.078182411074,82.7767072405916,230.080697217362));
#20316=CARTESIAN_POINT('Ctrl Pts',(262.074405587126,82.763042642054,230.080349199255));
#20317=CARTESIAN_POINT('Ctrl Pts',(262.070652408175,82.7493764437098,230.080014525542));
#20318=CARTESIAN_POINT('Ctrl Pts',(261.979457301859,82.417313830294,230.0718825912));
#20319=CARTESIAN_POINT('Ctrl Pts',(261.901916508769,82.0840986416051,230.071504242517));
#20320=CARTESIAN_POINT('Ctrl Pts',(261.837665799815,81.7496382953417,230.078654173433));
#20321=CARTESIAN_POINT('Ctrl Pts',(261.773415090861,81.4151779490784,230.08580410435));
#20322=CARTESIAN_POINT('Ctrl Pts',(261.722454613692,81.0794724258029,230.100482419413));
#20323=CARTESIAN_POINT('Ctrl Pts',(261.684465227673,80.7424242137756,230.12248991823));
#20324=CARTESIAN_POINT('Ctrl Pts',(261.64549555144,80.3966787023512,230.145065305555));
#20325=CARTESIAN_POINT('Ctrl Pts',(261.620197803172,80.0493109343409,230.175394454572));
#20326=CARTESIAN_POINT('Ctrl Pts',(261.608673985579,79.7006034747511,230.213303729148));
#20327=CARTESIAN_POINT('Ctrl Pts',(261.597663923829,79.3674421216154,230.24952292913));
#20328=CARTESIAN_POINT('Ctrl Pts',(261.599227267589,79.0330576316676,230.292661700132));
#20329=CARTESIAN_POINT('Ctrl Pts',(261.613491303076,78.6976913253862,230.342590522417));
#20330=CARTESIAN_POINT('Origin',(290.197052756605,75.7062702018219,253.073593133703));
#20331=CARTESIAN_POINT('',(259.737667058827,79.3576729844988,275.837689461751));
#20332=CARTESIAN_POINT('',(289.458803205568,72.5045665978414,275.837689461751));
#20333=CARTESIAN_POINT('',(261.613491303351,78.6976913251852,275.804595744969));
#20334=CARTESIAN_POINT('Ctrl Pts',(259.737667058827,79.3576729844988,275.837689461751));
#20335=CARTESIAN_POINT('Ctrl Pts',(260.387795558813,79.2077662059219,275.837689461751));
#20336=CARTESIAN_POINT('Ctrl Pts',(261.012965195301,78.9874393341337,275.827340932196));
#20337=CARTESIAN_POINT('Ctrl Pts',(261.613491303076,78.6976913253861,275.804595744989));
#20338=CARTESIAN_POINT('',(269.82981977108,91.6423159687713,273.29846276181));
#20339=CARTESIAN_POINT('Ctrl Pts',(261.613491303076,78.6976913253861,275.804595744989));
#20340=CARTESIAN_POINT('Ctrl Pts',(261.603419886992,78.9344836142266,275.839849018459));
#20341=CARTESIAN_POINT('Ctrl Pts',(261.599669504006,79.1715618901526,275.871823022698));
#20342=CARTESIAN_POINT('Ctrl Pts',(261.602281421227,79.4088047836705,275.900417526435));
#20343=CARTESIAN_POINT('Ctrl Pts',(261.604869397012,79.6438730541296,275.928749926358));
#20344=CARTESIAN_POINT('Ctrl Pts',(261.613703439758,79.8791034159246,275.953764712688));
#20345=CARTESIAN_POINT('Ctrl Pts',(261.628866516772,80.1143982791075,275.975346498954));
#20346=CARTESIAN_POINT('Ctrl Pts',(261.642231690708,80.321793965998,275.994369308575));
#20347=CARTESIAN_POINT('Ctrl Pts',(261.660514524517,80.5292402432758,276.010724810371));
#20348=CARTESIAN_POINT('Ctrl Pts',(261.683801145841,80.7366793730089,276.024320275013));
#20349=CARTESIAN_POINT('Ctrl Pts',(261.685335442275,80.7503470112872,276.025216045705));
#20350=CARTESIAN_POINT('Ctrl Pts',(261.68689089014,80.7640100348414,276.026099586327));
#20351=CARTESIAN_POINT('Ctrl Pts',(261.688467484406,80.7776684911368,276.026970901121));
#20352=CARTESIAN_POINT('Ctrl Pts',(261.721888633146,81.0672048095263,276.045441310387));
#20353=CARTESIAN_POINT('Ctrl Pts',(261.764898719889,81.3553538370425,276.058458227586));
#20354=CARTESIAN_POINT('Ctrl Pts',(261.817479571976,81.6419481819336,276.065959232372));
#20355=CARTESIAN_POINT('Ctrl Pts',(261.82457895601,81.6806437000837,276.066972006253));
#20356=CARTESIAN_POINT('Ctrl Pts',(261.831852749041,81.7193108918648,276.067884263523));
#20357=CARTESIAN_POINT('Ctrl Pts',(261.839300844835,81.7579493597271,276.068695886441));
#20358=CARTESIAN_POINT('Ctrl Pts',(261.842753889475,81.7758627107472,276.069072166533));
#20359=CARTESIAN_POINT('Ctrl Pts',(261.846245375141,81.793772849323,276.069426653246));
#20360=CARTESIAN_POINT('Ctrl Pts',(261.849775083155,81.8116789582788,276.069759361994));
#20361=CARTESIAN_POINT('Ctrl Pts',(261.890544284871,82.018499965865,276.073602249275));
#20362=CARTESIAN_POINT('Ctrl Pts',(261.936461352576,82.2249739958989,276.074541167105));
#20363=CARTESIAN_POINT('Ctrl Pts',(261.987165998336,82.4296701642412,276.072593815571));
#20364=CARTESIAN_POINT('Ctrl Pts',(262.014944591286,82.5418131731036,276.071526957007));
#20365=CARTESIAN_POINT('Ctrl Pts',(262.044159320794,82.6534226072953,276.069594266407));
#20366=CARTESIAN_POINT('Ctrl Pts',(262.074745527312,82.7642652337524,276.066801927027));
#20367=CARTESIAN_POINT('Ctrl Pts',(262.080807575631,82.7862337428924,276.066248497943));
#20368=CARTESIAN_POINT('Ctrl Pts',(262.086923423206,82.8081751913569,276.065661660633));
#20369=CARTESIAN_POINT('Ctrl Pts',(262.093092874244,82.830089346474,276.065041526113));
#20370=CARTESIAN_POINT('Ctrl Pts',(262.239688206997,83.3508022659059,276.050306207561));
#20371=CARTESIAN_POINT('Ctrl Pts',(262.41667027088,83.8566774376446,276.016757809987));
#20372=CARTESIAN_POINT('Ctrl Pts',(262.622710540289,84.3484094919605,275.965660356875));
#20373=CARTESIAN_POINT('Ctrl Pts',(262.669732754181,84.4606318740334,275.95399896963));
#20374=CARTESIAN_POINT('Ctrl Pts',(262.718268563109,84.5721175147771,275.941423440521));
#20375=CARTESIAN_POINT('Ctrl Pts',(262.768302408475,84.6828744721218,275.927948585287));
#20376=CARTESIAN_POINT('Ctrl Pts',(262.780537482962,84.7099585311849,275.924653498605));
#20377=CARTESIAN_POINT('Ctrl Pts',(262.79286252355,84.7369988532753,275.921304525794));
#20378=CARTESIAN_POINT('Ctrl Pts',(262.805277497977,84.7639954743981,275.917901836472));
#20379=CARTESIAN_POINT('Ctrl Pts',(262.911345432536,84.994642412861,275.888830795653));
#20380=CARTESIAN_POINT('Ctrl Pts',(263.024017624507,85.2221756769784,275.855827045657));
#20381=CARTESIAN_POINT('Ctrl Pts',(263.143170912963,85.446437155884,275.819023904925));
#20382=CARTESIAN_POINT('Ctrl Pts',(263.169270686232,85.4955602126477,275.810962410012));
#20383=CARTESIAN_POINT('Ctrl Pts',(263.195681264233,85.5445263664599,275.802718709764));
#20384=CARTESIAN_POINT('Ctrl Pts',(263.222401085225,85.593334085818,275.794294354551));
#20385=CARTESIAN_POINT('Ctrl Pts',(263.237950817452,85.6217379799495,275.78939175929));
#20386=CARTESIAN_POINT('Ctrl Pts',(263.253611058094,85.6500969358685,275.784425951054));
#20387=CARTESIAN_POINT('Ctrl Pts',(263.269379805331,85.6784078046249,275.779397861218));
#20388=CARTESIAN_POINT('Ctrl Pts',(263.369197762317,85.8576188121514,275.747569482756));
#20389=CARTESIAN_POINT('Ctrl Pts',(263.473528417736,86.0351791520541,275.71319386757));
#20390=CARTESIAN_POINT('Ctrl Pts',(263.581823584891,86.2101512509082,275.67651972138));
#20391=CARTESIAN_POINT('Ctrl Pts',(263.636102278675,86.2978491346089,275.658138247828));
#20392=CARTESIAN_POINT('Ctrl Pts',(263.691376235654,86.384897129559,275.639179737817));
#20393=CARTESIAN_POINT('Ctrl Pts',(263.747572835325,86.4711798102641,275.619677600556));
#20394=CARTESIAN_POINT('Ctrl Pts',(263.766352924537,86.5000142317514,275.613160268907));
#20395=CARTESIAN_POINT('Ctrl Pts',(263.785222875216,86.5287501659856,275.60658677669));
#20396=CARTESIAN_POINT('Ctrl Pts',(263.804181798426,86.5573870000339,275.599957983946));
#20397=CARTESIAN_POINT('Ctrl Pts',(263.99926400509,86.8520522991073,275.531749494383));
#20398=CARTESIAN_POINT('Ctrl Pts',(264.203747945169,87.1363444639111,275.457666020119));
#20399=CARTESIAN_POINT('Ctrl Pts',(264.417436929835,87.4107743914387,275.378347943292));
#20400=CARTESIAN_POINT('Ctrl Pts',(264.635378479409,87.6906656724454,275.297451379531));
#20401=CARTESIAN_POINT('Ctrl Pts',(264.862895108527,87.9602981495343,275.211109589539));
#20402=CARTESIAN_POINT('Ctrl Pts',(265.099806030715,88.2201770788809,275.119971097024));
#20403=CARTESIAN_POINT('Ctrl Pts',(265.34425799555,88.488328138829,275.025931601665));
#20404=CARTESIAN_POINT('Ctrl Pts',(265.598711781157,88.7460947841456,274.926785005734));
#20405=CARTESIAN_POINT('Ctrl Pts',(265.862998468363,88.993994667417,274.823214078989));
#20406=CARTESIAN_POINT('Ctrl Pts',(266.044076214604,89.1638448881395,274.752251783501));
#20407=CARTESIAN_POINT('Ctrl Pts',(266.22977053553,89.3290624729336,274.679211910719));
#20408=CARTESIAN_POINT('Ctrl Pts',(266.420034893768,89.4898045719229,274.604307092073));
#20409=CARTESIAN_POINT('Ctrl Pts',(266.441020935556,89.5075343266592,274.596045136609));
#20410=CARTESIAN_POINT('Ctrl Pts',(266.462047068505,89.5251961709156,274.587766503733));
#20411=CARTESIAN_POINT('Ctrl Pts',(266.483113285084,89.5427902642426,274.579471564047));
#20412=CARTESIAN_POINT('Ctrl Pts',(266.739576892666,89.7569836686354,274.47848759531));
#20413=CARTESIAN_POINT('Ctrl Pts',(267.001631199948,89.9608895027467,274.375211039575));
#20414=CARTESIAN_POINT('Ctrl Pts',(267.269275334688,90.1548901204229,274.270292993316));
#20415=CARTESIAN_POINT('Ctrl Pts',(267.540201437032,90.3512696571924,274.164088396806));
#20416=CARTESIAN_POINT('Ctrl Pts',(267.816855288512,90.537499489122,274.056201405317));
#20417=CARTESIAN_POINT('Ctrl Pts',(268.099260614184,90.7139333766602,273.94728207569));
#20418=CARTESIAN_POINT('Ctrl Pts',(268.389137035801,90.8950348620868,273.835481260879));
#20419=CARTESIAN_POINT('Ctrl Pts',(268.685073201994,91.0658152717133,273.722592360192));
#20420=CARTESIAN_POINT('Ctrl Pts',(268.98712122822,91.2266125215922,273.609298017563));
#20421=CARTESIAN_POINT('Ctrl Pts',(269.262905643181,91.3734281655784,273.505854818842));
#20422=CARTESIAN_POINT('Ctrl Pts',(269.543785584644,91.5119206718048,273.402073104508));
#20423=CARTESIAN_POINT('Ctrl Pts',(269.82981977108,91.6423159687712,273.29846276181));
#20424=CARTESIAN_POINT('',(292.657884593393,86.3786155484235,273.29846276181));
#20425=CARTESIAN_POINT('Origin',(255.074370622327,80.7261481941816,260.573593133704));
#20426=CARTESIAN_POINT('Origin',(139.64640668573,110.42027268846,253.073593133703));
#20427=CARTESIAN_POINT('Origin',(289.522998818702,72.7829756068832,273.85820282453));
#20428=CARTESIAN_POINT('Origin',(259.80186267196,79.6360819935406,273.85820282453));
#20429=CARTESIAN_POINT('Ctrl Pts',(259.352493380025,77.6872189302482,273.85820282453));
#20430=CARTESIAN_POINT('Ctrl Pts',(259.352493380025,77.6872189302482,275.590253632099));
#20431=CARTESIAN_POINT('Ctrl Pts',(259.737667058827,79.3576729844988,275.837689461751));
#20432=CARTESIAN_POINT('Ctrl Pts',(259.950395610532,77.5493544968614,273.858202824316));
#20433=CARTESIAN_POINT('Ctrl Pts',(259.969638708473,77.5449174176954,275.590253631842));
#20434=CARTESIAN_POINT('Ctrl Pts',(260.489866638764,79.1842306313116,275.837689461527));
#20435=CARTESIAN_POINT('Ctrl Pts',(260.520304163086,77.34418247573,273.845727756372));
#20436=CARTESIAN_POINT('Ctrl Pts',(260.55632630418,77.3317737998276,275.572104967451));
#20437=CARTESIAN_POINT('Ctrl Pts',(261.204913401109,78.9177192700401,275.824026291386));
#20438=CARTESIAN_POINT('Ctrl Pts',(261.334314889648,76.9392458488615,273.803773140294));
#20439=CARTESIAN_POINT('Ctrl Pts',(261.39984718193,76.9039004839026,275.514566262518));
#20440=CARTESIAN_POINT('Ctrl Pts',(262.223292632644,78.3835679167525,275.778075998304));
#20441=CARTESIAN_POINT('Ctrl Pts',(261.600168265855,76.7869681618089,273.78564891822));
#20442=CARTESIAN_POINT('Ctrl Pts',(261.675379825811,76.7425527899067,275.490123794013));
#20443=CARTESIAN_POINT('Ctrl Pts',(262.555366780798,78.1816425648451,275.758225659285));
#20444=CARTESIAN_POINT('Ctrl Pts',(262.110942369245,76.4526422432437,273.739442671591));
#20445=CARTESIAN_POINT('Ctrl Pts',(262.205789159906,76.3857612367168,275.429609986423));
#20446=CARTESIAN_POINT('Ctrl Pts',(263.192272886497,77.7364025768395,275.707618818374));
#20447=CARTESIAN_POINT('Ctrl Pts',(262.353991061074,76.2720769658325,273.711582345508));
#20448=CARTESIAN_POINT('Ctrl Pts',(262.458640311379,76.1920833314006,275.393879863165));
#20449=CARTESIAN_POINT('Ctrl Pts',(263.494777280233,77.4950731950082,275.67710512717));
#20450=CARTESIAN_POINT('Ctrl Pts',(262.816166800432,75.8852869421232,273.643922776295));
#20451=CARTESIAN_POINT('Ctrl Pts',(262.93982714268,75.7742357891089,275.309622118513));
#20452=CARTESIAN_POINT('Ctrl Pts',(264.068873292152,76.9765864414364,275.603001790289));
#20453=CARTESIAN_POINT('Ctrl Pts',(263.035290733386,75.6790579795937,273.604129294606));
#20454=CARTESIAN_POINT('Ctrl Pts',(263.168240525528,75.5501498442423,275.261138675086));
#20455=CARTESIAN_POINT('Ctrl Pts',(264.340460862288,76.6994232039232,275.559418452284));
#20456=CARTESIAN_POINT('Ctrl Pts',(263.449407025878,75.2411080436662,273.509217640416));
#20457=CARTESIAN_POINT('Ctrl Pts',(263.599273270717,75.0709585050466,275.148629692437));
#20458=CARTESIAN_POINT('Ctrl Pts',(264.852462244811,76.1094929549171,275.455467593939));
#20459=CARTESIAN_POINT('Ctrl Pts',(263.645621061591,75.0075891196608,273.453599168673));
#20460=CARTESIAN_POINT('Ctrl Pts',(263.803351197742,74.8137915708697,275.084050570573));
#20461=CARTESIAN_POINT('Ctrl Pts',(265.094373229636,75.7942915062644,275.394552123933));
#20462=CARTESIAN_POINT('Ctrl Pts',(264.18452429865,74.2844949805711,273.261503260181));
#20463=CARTESIAN_POINT('Ctrl Pts',(264.360159533119,74.0132571206072,274.86652779898));
#20464=CARTESIAN_POINT('Ctrl Pts',(265.756639414063,74.8164649195017,275.184161368368));
#20465=CARTESIAN_POINT('Ctrl Pts',(264.479839828946,73.7723884511662,273.100414005911));
#20466=CARTESIAN_POINT('Ctrl Pts',(264.662785788954,73.4369654880319,274.689319013975));
#20467=CARTESIAN_POINT('Ctrl Pts',(266.116520847396,74.1216801997296,275.007727891442));
#20468=CARTESIAN_POINT('Ctrl Pts',(264.714335805196,73.2350168556771,272.892880023885));
#20469=CARTESIAN_POINT('Ctrl Pts',(264.891797790303,72.8283445041923,274.469890825203));
#20470=CARTESIAN_POINT('Ctrl Pts',(266.39885077907,73.3906559987533,274.780431156283));
#20471=CARTESIAN_POINT('Ctrl Pts',(261.613491303169,78.6976913251228,275.804595744953));
#20472=CARTESIAN_POINT('Ctrl Pts',(261.640463121467,78.6217294719184,275.79410972222));
#20473=CARTESIAN_POINT('Ctrl Pts',(261.668927419666,78.5471358444608,275.781382564128));
#20474=CARTESIAN_POINT('Ctrl Pts',(261.698675179246,78.4737068307562,275.76674155216));
#20475=CARTESIAN_POINT('Ctrl Pts',(261.729027718461,78.3987849862377,275.751802884637));
#20476=CARTESIAN_POINT('Ctrl Pts',(261.76071647419,78.3250757793365,275.734871638552));
#20477=CARTESIAN_POINT('Ctrl Pts',(261.793541102325,78.2523960866447,275.716256908152));
#20478=CARTESIAN_POINT('Ctrl Pts',(261.827408822181,78.1774067992964,275.697050644129));
#20479=CARTESIAN_POINT('Ctrl Pts',(261.862485754497,78.1035136413755,275.676052146321));
#20480=CARTESIAN_POINT('Ctrl Pts',(261.89857443723,78.0305479237867,275.653561505271));
#20481=CARTESIAN_POINT('Ctrl Pts',(261.916261738067,77.9947869455509,275.642538694125));
#20482=CARTESIAN_POINT('Ctrl Pts',(261.934192403458,77.9592492137772,275.63115687955));
#20483=CARTESIAN_POINT('Ctrl Pts',(261.952345067313,77.9239174154688,275.619448165681));
#20484=CARTESIAN_POINT('Ctrl Pts',(261.985756831217,77.8588857643113,275.597897125759));
#20485=CARTESIAN_POINT('Ctrl Pts',(262.01988412855,77.794622083521,275.575265396718));
#20486=CARTESIAN_POINT('Ctrl Pts',(262.054660477631,77.7309198561505,275.55169804487));
#20487=CARTESIAN_POINT('Ctrl Pts',(262.090751989985,77.6648085538752,275.527239428803));
#20488=CARTESIAN_POINT('Ctrl Pts',(262.127542591829,77.5993022921848,275.501772939713));
#20489=CARTESIAN_POINT('Ctrl Pts',(262.164991025203,77.5341799597694,275.475416808112));
#20490=CARTESIAN_POINT('Ctrl Pts',(262.173788840419,77.5188806749813,275.469224923572));
#20491=CARTESIAN_POINT('Ctrl Pts',(262.182623101299,77.5036026092372,275.462983758236));
#20492=CARTESIAN_POINT('Ctrl Pts',(262.191493522389,77.4883429401822,275.456694524797));
#20493=CARTESIAN_POINT('Ctrl Pts',(262.231953816496,77.418739626913,275.428007697861));
#20494=CARTESIAN_POINT('Ctrl Pts',(262.272838079584,77.350048000437,275.398535810711));
#20495=CARTESIAN_POINT('Ctrl Pts',(262.314099531327,77.2819808754804,275.368314912438));
#20496=CARTESIAN_POINT('Ctrl Pts',(262.328401654566,77.258387318577,275.357839686938));
#20497=CARTESIAN_POINT('Ctrl Pts',(262.342749438049,77.2348688922053,275.347274161733));
#20498=CARTESIAN_POINT('Ctrl Pts',(262.357141963554,77.2114139037108,275.336618888011));
#20499=CARTESIAN_POINT('Ctrl Pts',(262.410079203,77.1251439616009,275.297427658077));
#20500=CARTESIAN_POINT('Ctrl Pts',(262.463569962561,77.0398179251102,275.257065801432));
#20501=CARTESIAN_POINT('Ctrl Pts',(262.517379093069,76.9552242466752,275.215708031544));
#20502=CARTESIAN_POINT('Ctrl Pts',(262.572627824017,76.8683673631756,275.173243782827));
#20503=CARTESIAN_POINT('Ctrl Pts',(262.628212404354,76.7822827727532,275.129729548656));
#20504=CARTESIAN_POINT('Ctrl Pts',(262.683920945102,76.6967676750229,275.085326562061));
#20505=CARTESIAN_POINT('Ctrl Pts',(262.742307773582,76.6071412860253,275.038788822471));
#20506=CARTESIAN_POINT('Ctrl Pts',(262.800830872367,76.518140639542,274.991274835981));
#20507=CARTESIAN_POINT('Ctrl Pts',(262.85929021809,76.4295576324981,274.942940292671));
#20508=CARTESIAN_POINT('Ctrl Pts',(262.908026182039,76.3557083927509,274.90264510067));
#20509=CARTESIAN_POINT('Ctrl Pts',(262.956718746885,76.2821499717718,274.861779015391));
#20510=CARTESIAN_POINT('Ctrl Pts',(263.005272555425,76.2087727973901,274.820417589951));
#20511=CARTESIAN_POINT('Ctrl Pts',(263.060542637539,76.1252456225852,274.773334787403));
#20512=CARTESIAN_POINT('Ctrl Pts',(263.115708369896,76.0418382064472,274.725490781205));
#20513=CARTESIAN_POINT('Ctrl Pts',(263.170530251593,75.958601926688,274.677015542267));
#20514=CARTESIAN_POINT('Ctrl Pts',(263.18715735304,75.9333569328139,274.662313334125));
#20515=CARTESIAN_POINT('Ctrl Pts',(263.203753124808,75.9081275516313,274.647552890128));
#20516=CARTESIAN_POINT('Ctrl Pts',(263.220311635213,75.8829148882721,274.632737403038));
#20517=CARTESIAN_POINT('Ctrl Pts',(263.280731719076,75.7909168040654,274.578677409079));
#20518=CARTESIAN_POINT('Ctrl Pts',(263.340785418365,75.6989423502989,274.523770259114));
#20519=CARTESIAN_POINT('Ctrl Pts',(263.400202842949,75.6070406003285,274.468146294033));
#20520=CARTESIAN_POINT('Ctrl Pts',(263.417872769097,75.5797102818875,274.451604490649));
#20521=CARTESIAN_POINT('Ctrl Pts',(263.4354867097,75.5523862658522,274.434999122649));
#20522=CARTESIAN_POINT('Ctrl Pts',(263.453038257251,75.5250695291328,274.418333198669));
#20523=CARTESIAN_POINT('Ctrl Pts',(263.531183974767,75.4034457244507,274.344130591536));
#20524=CARTESIAN_POINT('Ctrl Pts',(263.60801194364,75.2820831684112,274.268811207293));
#20525=CARTESIAN_POINT('Ctrl Pts',(263.683293494855,75.1607510839154,274.192319481584));
#20526=CARTESIAN_POINT('Ctrl Pts',(263.756243034221,75.0431775279582,274.118197255543));
#20527=CARTESIAN_POINT('Ctrl Pts',(263.827741740394,74.9256328135397,274.042974155082));
#20528=CARTESIAN_POINT('Ctrl Pts',(263.897622681191,74.8078999833618,273.966578931842));
#20529=CARTESIAN_POINT('Ctrl Pts',(263.941871575824,74.7333510786387,273.918205167192));
#20530=CARTESIAN_POINT('Ctrl Pts',(263.985462003184,74.6587045073954,273.869359764373));
#20531=CARTESIAN_POINT('Ctrl Pts',(264.028363007675,74.583948413358,273.820012956539));
#20532=CARTESIAN_POINT('Ctrl Pts',(264.106301190796,74.4481391423252,273.730364693264));
#20533=CARTESIAN_POINT('Ctrl Pts',(264.181908511619,74.3120674435541,273.639133544911));
#20534=CARTESIAN_POINT('Ctrl Pts',(264.25497364732,74.1757277968292,273.54618930162));
#20535=CARTESIAN_POINT('Ctrl Pts',(264.298661947877,74.0942053660987,273.490614560029));
#20536=CARTESIAN_POINT('Ctrl Pts',(264.341442030647,74.0125863394151,273.434426941907));
#20537=CARTESIAN_POINT('Ctrl Pts',(264.383272984049,73.9308629539767,273.377594728271));
#20538=CARTESIAN_POINT('Ctrl Pts',(264.432025871625,73.8356164750296,273.311358262288));
#20539=CARTESIAN_POINT('Ctrl Pts',(264.479623489581,73.7399603004325,273.244059730206));
#20540=CARTESIAN_POINT('Ctrl Pts',(264.525812267634,73.644243708693,273.175895849824));
#20541=CARTESIAN_POINT('Ctrl Pts',(264.571084485189,73.5504264970762,273.109084599295));
#20542=CARTESIAN_POINT('Ctrl Pts',(264.615002988964,73.4565515061618,273.041442047184));
#20543=CARTESIAN_POINT('Ctrl Pts',(264.657365195295,73.3629565418885,272.973187172579));
#20544=CARTESIAN_POINT('Ctrl Pts',(264.670885765522,73.3330842241583,272.951402546487));
#20545=CARTESIAN_POINT('Ctrl Pts',(264.684248094534,73.3032404851218,272.929555803375));
#20546=CARTESIAN_POINT('Ctrl Pts',(264.697446445794,73.2734364402348,272.907654791342));
#20547=CARTESIAN_POINT('Ctrl Pts',(263.544486310321,78.4442745295379,277.78120466771));
#20548=CARTESIAN_POINT('Ctrl Pts',(263.538250261041,78.7291375341272,275.876052151847));
#20549=CARTESIAN_POINT('Ctrl Pts',(261.613491303076,78.6976913253861,275.804595744989));
#20550=CARTESIAN_POINT('Ctrl Pts',(263.557302515182,77.8588297294296,277.680650907661));
#20551=CARTESIAN_POINT('Ctrl Pts',(263.533654545806,78.3947691062696,275.950105354397));
#20552=CARTESIAN_POINT('Ctrl Pts',(261.754727069594,78.2999231642985,275.749686526725));
#20553=CARTESIAN_POINT('Ctrl Pts',(263.606591880381,77.3148820941794,277.451481936637));
#20554=CARTESIAN_POINT('Ctrl Pts',(263.538547887186,77.9742246260938,275.962292428753));
#20555=CARTESIAN_POINT('Ctrl Pts',(261.949245797882,77.9050773398094,275.628452153648));
#20556=CARTESIAN_POINT('Ctrl Pts',(263.755975405511,76.2858158960412,276.814036792249));
#20557=CARTESIAN_POINT('Ctrl Pts',(263.624571850212,77.0153725191991,275.757092055883));
#20558=CARTESIAN_POINT('Ctrl Pts',(262.433710331132,77.0716088320336,275.284928037322));
#20559=CARTESIAN_POINT('Ctrl Pts',(263.852404590492,75.824998225666,276.4197615986));
#20560=CARTESIAN_POINT('Ctrl Pts',(263.698661733633,76.5115820479287,275.559759849144));
#20561=CARTESIAN_POINT('Ctrl Pts',(262.711999049714,76.6519825800893,275.070246533072));
#20562=CARTESIAN_POINT('Ctrl Pts',(264.014706007828,75.1891126872895,275.756206976135));
#20563=CARTESIAN_POINT('Ctrl Pts',(263.858168373587,75.7622723596492,275.132856736245));
#20564=CARTESIAN_POINT('Ctrl Pts',(263.151909041545,75.9871679741537,274.69550296854));
#20565=CARTESIAN_POINT('Ctrl Pts',(264.072112191271,74.9857513363534,275.521600607894));
#20566=CARTESIAN_POINT('Ctrl Pts',(263.917768744914,75.5167006386421,274.972965619438));
#20567=CARTESIAN_POINT('Ctrl Pts',(263.302835955358,75.7588393827117,274.560956346748));
#20568=CARTESIAN_POINT('Ctrl Pts',(264.190557682099,74.5984025565768,275.035373464112));
#20569=CARTESIAN_POINT('Ctrl Pts',(264.048271575533,75.0381564136266,274.623431382325));
#20570=CARTESIAN_POINT('Ctrl Pts',(263.603229270736,75.2913050055039,274.275702018227));
#20571=CARTESIAN_POINT('Ctrl Pts',(264.251478238831,74.4146529473688,274.784242803635));
#20572=CARTESIAN_POINT('Ctrl Pts',(264.119123197892,74.8037832321255,274.43390177169));
#20573=CARTESIAN_POINT('Ctrl Pts',(263.752412397567,75.0525305312594,274.125297564039));
#20574=CARTESIAN_POINT('Ctrl Pts',(264.437749904692,73.8878858378157,274.010861079826));
#20575=CARTESIAN_POINT('Ctrl Pts',(264.343108315133,74.1265992212334,273.83709802127));
#20576=CARTESIAN_POINT('Ctrl Pts',(264.188012233111,74.3186632559562,273.649114033831));
#20577=CARTESIAN_POINT('Ctrl Pts',(264.566427694471,73.5692983043154,273.468513234698));
#20578=CARTESIAN_POINT('Ctrl Pts',(264.514363032585,73.6868688639712,273.383107148469));
#20579=CARTESIAN_POINT('Ctrl Pts',(264.462022086354,73.8050633190648,273.298312058746));
#20580=CARTESIAN_POINT('Ctrl Pts',(264.697446473732,73.2734363771458,272.907654744982));
#20581=CARTESIAN_POINT('Ctrl Pts',(264.697446473732,73.2734363771458,272.907654744982));
#20582=CARTESIAN_POINT('Ctrl Pts',(264.697446473732,73.2734363771458,272.907654744982));
#20583=CARTESIAN_POINT('Origin',(261.544965371427,78.4005022217613,277.78120466771));
#20584=CARTESIAN_POINT('Ctrl Pts',(261.613491303076,78.6976913253861,275.804595744989));
#20585=CARTESIAN_POINT('Ctrl Pts',(263.538250261041,78.7291375341272,275.876052151847));
#20586=CARTESIAN_POINT('Ctrl Pts',(263.544486310321,78.4442745295379,277.78120466771));
#20587=CARTESIAN_POINT('Ctrl Pts',(261.584924963991,79.3693236611784,275.90458733896));
#20588=CARTESIAN_POINT('Ctrl Pts',(263.538751417713,79.3208320667281,275.951422448941));
#20589=CARTESIAN_POINT('Ctrl Pts',(263.530633522654,79.0770704776892,277.889891267409));
#20590=CARTESIAN_POINT('Ctrl Pts',(261.606888594957,80.0515359965378,275.97941629239));
#20591=CARTESIAN_POINT('Ctrl Pts',(263.577708183242,79.9084748007003,276.005543753781));
#20592=CARTESIAN_POINT('Ctrl Pts',(263.561159360681,79.7206789971068,277.971227001875));
#20593=CARTESIAN_POINT('Ctrl Pts',(261.722256160334,81.0792512150198,276.046772257573));
#20594=CARTESIAN_POINT('Ctrl Pts',(263.694408709898,80.7915012776091,276.054308283014));
#20595=CARTESIAN_POINT('Ctrl Pts',(263.679123147862,80.6916047864155,278.044440007458));
#20596=CARTESIAN_POINT('Ctrl Pts',(261.774083994414,81.4196746921591,276.061590187108));
#20597=CARTESIAN_POINT('Ctrl Pts',(263.742807893208,81.0834999396488,276.064954230829));
#20598=CARTESIAN_POINT('Ctrl Pts',(263.730106477294,81.0134428912567,278.060546452654));
#20599=CARTESIAN_POINT('Ctrl Pts',(261.904506161914,82.0962262854197,276.075801577687));
#20600=CARTESIAN_POINT('Ctrl Pts',(263.858611890859,81.6646469545893,276.07518727214));
#20601=CARTESIAN_POINT('Ctrl Pts',(263.855417008547,81.6535129221044,278.075993616262));
#20602=CARTESIAN_POINT('Ctrl Pts',(261.983448859087,82.4334104511011,276.075136798143));
#20603=CARTESIAN_POINT('Ctrl Pts',(263.926196279394,81.9540846684519,276.074711158139));
#20604=CARTESIAN_POINT('Ctrl Pts',(263.930066466954,81.9727463532846,278.075271029728));
#20605=CARTESIAN_POINT('Ctrl Pts',(262.257324061002,83.4259788289607,276.050132170168));
#20606=CARTESIAN_POINT('Ctrl Pts',(264.155346427456,82.8090535366488,276.056711404079));
#20607=CARTESIAN_POINT('Ctrl Pts',(264.186108538369,82.9131611918406,278.048092086594));
#20608=CARTESIAN_POINT('Ctrl Pts',(262.489246294873,84.0651482976787,276.003102117324));
#20609=CARTESIAN_POINT('Ctrl Pts',(264.342254943422,83.3613811113261,276.023184668261));
#20610=CARTESIAN_POINT('Ctrl Pts',(264.399590570473,83.519667383898,277.996972463593));
#20611=CARTESIAN_POINT('Ctrl Pts',(262.907828258109,84.991738509739,275.890371770625));
#20612=CARTESIAN_POINT('Ctrl Pts',(264.679770033545,84.1792123901588,275.94003272305));
#20613=CARTESIAN_POINT('Ctrl Pts',(264.781126806292,84.4002721698412,277.874439478249));
#20614=CARTESIAN_POINT('Ctrl Pts',(263.05918892757,85.2952200573854,275.845750061578));
#20615=CARTESIAN_POINT('Ctrl Pts',(264.801019872423,84.4481788348286,275.907041959933));
#20616=CARTESIAN_POINT('Ctrl Pts',(264.918568019719,84.6889288671942,277.825937620468));
#20617=CARTESIAN_POINT('Ctrl Pts',(263.385603217161,85.8914532581418,275.742838213459));
#20618=CARTESIAN_POINT('Ctrl Pts',(265.063276334391,84.9817577086832,275.829892444549));
#20619=CARTESIAN_POINT('Ctrl Pts',(265.21399891031,85.2565181212866,277.714076916101));
#20620=CARTESIAN_POINT('Ctrl Pts',(263.56129340771,86.1851653448694,275.68432430288));
#20621=CARTESIAN_POINT('Ctrl Pts',(265.204448884394,85.2468357118572,275.785699044745));
#20622=CARTESIAN_POINT('Ctrl Pts',(265.37256137918,85.536366807698,277.650474839131));
#20623=CARTESIAN_POINT('Ctrl Pts',(264.492544874104,87.615324849741,275.361080258794));
#20624=CARTESIAN_POINT('Ctrl Pts',(265.947933666804,86.5352397777713,275.540942276622));
#20625=CARTESIAN_POINT('Ctrl Pts',(266.21092639465,86.9002782684925,277.299122618297));
#20626=CARTESIAN_POINT('Ctrl Pts',(265.38578794737,88.6160477178875,275.011475602805));
#20627=CARTESIAN_POINT('Ctrl Pts',(266.671873010809,87.488473601431,275.267004329307));
#20628=CARTESIAN_POINT('Ctrl Pts',(267.008921214875,87.858651988119,276.919117556122));
#20629=CARTESIAN_POINT('Ctrl Pts',(267.454181512283,90.3636586447312,274.197111457415));
#20630=CARTESIAN_POINT('Ctrl Pts',(268.432540806735,89.2203249048919,274.579653206379));
#20631=CARTESIAN_POINT('Ctrl Pts',(268.84731196028,89.5407379995528,276.033939138256));
#20632=CARTESIAN_POINT('Ctrl Pts',(268.591652650856,91.0778688607264,273.746964814108));
#20633=CARTESIAN_POINT('Ctrl Pts',(269.421598796566,89.9678036643426,274.184725204187));
#20634=CARTESIAN_POINT('Ctrl Pts',(269.854099200818,90.2329609402673,275.544696281663));
#20635=CARTESIAN_POINT('Ctrl Pts',(269.82981977108,91.6423159687712,273.29846276181));
#20636=CARTESIAN_POINT('Ctrl Pts',(270.548229297884,90.584148594095,273.76942958616));
#20637=CARTESIAN_POINT('Ctrl Pts',(270.946701599761,90.7857513677001,275.057147077298));
#20638=CARTESIAN_POINT('Origin',(270.043805148192,92.5703459989105,275.057147077298));
#20639=CARTESIAN_POINT('Origin',(292.443899216281,85.4505855182842,271.539778446323));
#20640=CARTESIAN_POINT('Ctrl Pts',(273.255484225105,91.9275333837837,271.539778446323));
#20641=CARTESIAN_POINT('Ctrl Pts',(273.255484225105,91.9275333837837,271.563577454831));
#20642=CARTESIAN_POINT('Ctrl Pts',(273.253623088777,91.9275219541507,271.587173031064));
#20643=CARTESIAN_POINT('Ctrl Pts',(273.250054608046,91.9274970401005,271.610445617562));
#20644=CARTESIAN_POINT('Ctrl Pts',(273.246348308204,91.927471163839,271.634617019954));
#20645=CARTESIAN_POINT('Ctrl Pts',(273.240800633766,91.9274306765218,271.658439833613));
#20646=CARTESIAN_POINT('Ctrl Pts',(273.233641995375,91.9273743226171,271.681785099849));
#20647=CARTESIAN_POINT('Ctrl Pts',(273.225930813326,91.9273136190035,271.706932284006));
#20648=CARTESIAN_POINT('Ctrl Pts',(273.216350735339,91.9272344125153,271.731525078663));
#20649=CARTESIAN_POINT('Ctrl Pts',(273.205250501302,91.9271376093613,271.755411612847));
#20650=CARTESIAN_POINT('Ctrl Pts',(273.200790481524,91.9270987143272,271.765009105523));
#20651=CARTESIAN_POINT('Ctrl Pts',(273.196085663662,91.9270570129215,271.774492703576));
#20652=CARTESIAN_POINT('Ctrl Pts',(273.191160878823,91.9270127136269,271.7838530879));
#20653=CARTESIAN_POINT('Ctrl Pts',(273.179023642191,91.9269035370763,271.806921953493));
#20654=CARTESIAN_POINT('Ctrl Pts',(273.165569387512,91.926771118345,271.829276213771));
#20655=CARTESIAN_POINT('Ctrl Pts',(273.15105536297,91.9266146820572,271.850962154885));
#20656=CARTESIAN_POINT('Ctrl Pts',(273.144635935929,91.9265454916454,271.860553658356));
#20657=CARTESIAN_POINT('Ctrl Pts',(273.138008484825,91.9264716106079,271.870014436442));
#20658=CARTESIAN_POINT('Ctrl Pts',(273.131192071431,91.9263930063714,271.879348530148));
#20659=CARTESIAN_POINT('Ctrl Pts',(273.114779367358,91.9262037414313,271.901823358029));
#20660=CARTESIAN_POINT('Ctrl Pts',(273.097470710609,91.9259860378421,271.923396697541));
#20661=CARTESIAN_POINT('Ctrl Pts',(273.079474058163,91.9257382169349,271.944193936758));
#20662=CARTESIAN_POINT('Ctrl Pts',(273.066824949306,91.9255640337837,271.958811463188));
#20663=CARTESIAN_POINT('Ctrl Pts',(273.053834764524,91.9253749968506,271.973045197809));
#20664=CARTESIAN_POINT('Ctrl Pts',(273.040561221661,91.9251707917529,271.986933965451));
#20665=CARTESIAN_POINT('Ctrl Pts',(273.018634156517,91.9248334576647,272.009877343566));
#20666=CARTESIAN_POINT('Ctrl Pts',(272.995835208372,91.9244531801533,272.031985181632));
#20667=CARTESIAN_POINT('Ctrl Pts',(272.972361860486,91.9240268228059,272.053385779335));
#20668=CARTESIAN_POINT('Ctrl Pts',(272.947379075074,91.9235730488419,272.076162527787));
#20669=CARTESIAN_POINT('Ctrl Pts',(272.921632200933,91.9230671060948,272.098138107484));
#20670=CARTESIAN_POINT('Ctrl Pts',(272.895300190888,91.922505597192,272.119448758397));
#20671=CARTESIAN_POINT('Ctrl Pts',(272.869453101371,91.9219544288288,272.140366960269));
#20672=CARTESIAN_POINT('Ctrl Pts',(272.843041414019,91.9213497496453,272.160644248366));
#20673=CARTESIAN_POINT('Ctrl Pts',(272.816187852709,91.9206882763742,272.180394894944));
#20674=CARTESIAN_POINT('Ctrl Pts',(272.784505150081,91.9199078487541,272.203697348387));
#20675=CARTESIAN_POINT('Ctrl Pts',(272.752284224801,91.9190489558682,272.226182712055));
#20676=CARTESIAN_POINT('Ctrl Pts',(272.719622978659,91.9181105303922,272.247986020648));
#20677=CARTESIAN_POINT('Ctrl Pts',(272.695125012398,91.9174066529115,272.264339858342));
#20678=CARTESIAN_POINT('Ctrl Pts',(272.670377979989,91.9166579929307,272.28030961091));
#20679=CARTESIAN_POINT('Ctrl Pts',(272.645405122023,91.9158632887775,272.295946522169));
#20680=CARTESIAN_POINT('Ctrl Pts',(272.601097780684,91.9144533088616,272.32368984116));
#20681=CARTESIAN_POINT('Ctrl Pts',(272.556053140956,91.912897347606,272.350402646128));
#20682=CARTESIAN_POINT('Ctrl Pts',(272.510574130833,91.91119309357,272.376196962215));
#20683=CARTESIAN_POINT('Ctrl Pts',(272.472354806289,91.909760884779,272.397873804681));
#20684=CARTESIAN_POINT('Ctrl Pts',(272.433827432696,91.9082239447931,272.418901728127));
#20685=CARTESIAN_POINT('Ctrl Pts',(272.395144319412,91.906580460314,272.439340662118));
#20686=CARTESIAN_POINT('Ctrl Pts',(272.336857160485,91.9041040815303,272.470137753995));
#20687=CARTESIAN_POINT('Ctrl Pts',(272.278033409372,91.9013833209367,272.499695719002));
#20688=CARTESIAN_POINT('Ctrl Pts',(272.218759135935,91.8984096788626,272.528225589475));
#20689=CARTESIAN_POINT('Ctrl Pts',(272.155384374984,91.8952303255837,272.55872910502));
#20690=CARTESIAN_POINT('Ctrl Pts',(272.091494349814,91.8917620135632,272.588057263861));
#20691=CARTESIAN_POINT('Ctrl Pts',(272.027142805416,91.8879897181143,272.616435627212));
#20692=CARTESIAN_POINT('Ctrl Pts',(271.991734012766,91.8859140503332,272.632050537359));
#20693=CARTESIAN_POINT('Ctrl Pts',(271.956184629353,91.8837462565477,272.647377337366));
#20694=CARTESIAN_POINT('Ctrl Pts',(271.920498131808,91.8814830897533,272.662450052827));
#20695=CARTESIAN_POINT('Ctrl Pts',(271.862268990929,91.8777903132925,272.687043984212));
#20696=CARTESIAN_POINT('Ctrl Pts',(271.803630523397,91.8738384340663,272.71096347216));
#20697=CARTESIAN_POINT('Ctrl Pts',(271.744674380866,91.8696265270691,272.734262818706));
#20698=CARTESIAN_POINT('Ctrl Pts',(271.650842289134,91.8629230348331,272.771345068808));
#20699=CARTESIAN_POINT('Ctrl Pts',(271.556130751135,91.8555536840876,272.806886942222));
#20700=CARTESIAN_POINT('Ctrl Pts',(271.461255325209,91.8475267985236,272.840905168818));
#20701=CARTESIAN_POINT('Ctrl Pts',(271.445179827524,91.8461667394879,272.846669147399));
#20702=CARTESIAN_POINT('Ctrl Pts',(271.429099510396,91.8447877834954,272.852389348935));
#20703=CARTESIAN_POINT('Ctrl Pts',(271.413017727445,91.8433899471151,272.858065811931));
#20704=CARTESIAN_POINT('Ctrl Pts',(271.293504536816,91.8330018025733,272.900250948124));
#20705=CARTESIAN_POINT('Ctrl Pts',(271.173507435133,91.8215530737852,272.940190217739));
#20706=CARTESIAN_POINT('Ctrl Pts',(271.052959917239,91.8089715978704,272.978194428691));
#20707=CARTESIAN_POINT('Ctrl Pts',(270.999522572895,91.8033943726187,272.995041263389));
#20708=CARTESIAN_POINT('Ctrl Pts',(270.945976758625,91.7975942994658,273.011507245252));
#20709=CARTESIAN_POINT('Ctrl Pts',(270.892315466622,91.7915637910068,273.027616795162));
#20710=CARTESIAN_POINT('Ctrl Pts',(270.860374894621,91.7879742782976,273.037205610854));
#20711=CARTESIAN_POINT('Ctrl Pts',(270.828394131352,91.7843034378172,273.046670107705));
#20712=CARTESIAN_POINT('Ctrl Pts',(270.796369186396,91.7805492689741,273.056012079442));
#20713=CARTESIAN_POINT('Ctrl Pts',(270.521104434134,91.7482809744325,273.136309345819));
#20714=CARTESIAN_POINT('Ctrl Pts',(270.243771310296,91.7099651949295,273.207231978851));
#20715=CARTESIAN_POINT('Ctrl Pts',(269.965387262019,91.6648266164728,273.269078101933));
#20716=CARTESIAN_POINT('Ctrl Pts',(269.920224430833,91.6575036897053,273.279111528897));
#20717=CARTESIAN_POINT('Ctrl Pts',(269.875033852327,91.6500012300741,273.28890601228));
#20718=CARTESIAN_POINT('Ctrl Pts',(269.82981977108,91.6423159687712,273.29846276181));
#20719=CARTESIAN_POINT('Ctrl Pts',(274.135356630693,91.9232791773928,271.539778446323));
#20720=CARTESIAN_POINT('Ctrl Pts',(273.694940779298,91.8262033907668,271.539778446323));
#20721=CARTESIAN_POINT('Ctrl Pts',(273.255484225105,91.9275333837837,271.539778446323));
#20722=CARTESIAN_POINT('Ctrl Pts',(274.135356618139,91.9232791746256,271.77352759202));
#20723=CARTESIAN_POINT('Ctrl Pts',(273.694940766237,91.8262033874431,271.712138594175));
#20724=CARTESIAN_POINT('Ctrl Pts',(273.255484212108,91.9275333867805,271.656653018791));
#20725=CARTESIAN_POINT('Ctrl Pts',(274.094104920322,91.9143299491368,272.001710787058));
#20726=CARTESIAN_POINT('Ctrl Pts',(273.651729880129,91.8153819562333,271.880756949373));
#20727=CARTESIAN_POINT('Ctrl Pts',(273.210441477653,91.927321339897,271.77074461716));
#20728=CARTESIAN_POINT('Ctrl Pts',(273.948712475437,91.8809612331079,272.43610810231));
#20729=CARTESIAN_POINT('Ctrl Pts',(273.500699311358,91.7755432830053,272.197958934196));
#20730=CARTESIAN_POINT('Ctrl Pts',(273.051917078416,91.9254721937242,271.987943273847));
#20731=CARTESIAN_POINT('Ctrl Pts',(273.848753385412,91.8573753781329,272.634456464127));
#20732=CARTESIAN_POINT('Ctrl Pts',(273.396675272924,91.7473695895106,272.341448843629));
#20733=CARTESIAN_POINT('Ctrl Pts',(272.943010608921,91.9238122517172,272.087117455614));
#20734=CARTESIAN_POINT('Ctrl Pts',(273.61549231008,91.7983990370043,273.007566223003));
#20735=CARTESIAN_POINT('Ctrl Pts',(273.155975276006,91.6778806512037,272.606580240907));
#20736=CARTESIAN_POINT('Ctrl Pts',(272.689365096497,91.9175643010313,272.273672334273));
#20737=CARTESIAN_POINT('Ctrl Pts',(273.48331851805,91.7632558189231,273.179638632332));
#20738=CARTESIAN_POINT('Ctrl Pts',(273.019825191783,91.636639842145,272.726492502695));
#20739=CARTESIAN_POINT('Ctrl Pts',(272.545857611411,91.9129836201679,272.359708539774));
#20740=CARTESIAN_POINT('Ctrl Pts',(273.205089743305,91.6840327233082,273.498166259421));
#20741=CARTESIAN_POINT('Ctrl Pts',(272.735652702075,91.5449382008264,272.94309386566));
#20742=CARTESIAN_POINT('Ctrl Pts',(272.244430498303,91.9001776457436,272.518972352425));
#20743=CARTESIAN_POINT('Ctrl Pts',(273.057913590941,91.6396897520155,273.645915370351));
#20744=CARTESIAN_POINT('Ctrl Pts',(272.58594546409,91.4939300491432,273.040692149937));
#20745=CARTESIAN_POINT('Ctrl Pts',(272.085289161225,91.8919346167594,272.592846908584));
#20746=CARTESIAN_POINT('Ctrl Pts',(272.752379380603,91.5413516256883,273.924324537817));
#20747=CARTESIAN_POINT('Ctrl Pts',(272.27815788873,91.3824825706594,273.218316332999));
#20748=CARTESIAN_POINT('Ctrl Pts',(271.755705227879,91.8710331819526,272.732051491823));
#20749=CARTESIAN_POINT('Ctrl Pts',(272.593678387909,91.4872118120189,274.055012603804));
#20750=CARTESIAN_POINT('Ctrl Pts',(272.119348482168,91.321650261883,273.298198175737));
#20751=CARTESIAN_POINT('Ctrl Pts',(271.584897011395,91.8583306460472,272.797395525323));
#20752=CARTESIAN_POINT('Ctrl Pts',(272.273457666484,91.3709349540835,274.297680104029));
#20753=CARTESIAN_POINT('Ctrl Pts',(271.80251742236,91.1931416236028,273.439263812478));
#20754=CARTESIAN_POINT('Ctrl Pts',(271.241131095768,91.8284570802143,272.918729274917));
#20755=CARTESIAN_POINT('Ctrl Pts',(272.111164141465,91.3085699747133,274.410345911472));
#20756=CARTESIAN_POINT('Ctrl Pts',(271.64342889865,91.1249694608679,273.500705767743));
#20757=CARTESIAN_POINT('Ctrl Pts',(271.067336037362,91.8112458522357,272.975062179002));
#20758=CARTESIAN_POINT('Ctrl Pts',(271.619489127284,91.1082362789725,274.725628850557));
#20759=CARTESIAN_POINT('Ctrl Pts',(271.163441768428,90.9080618135687,273.661531752826));
#20760=CARTESIAN_POINT('Ctrl Pts',(270.542249033313,91.7522310661092,273.13270364823));
#20761=CARTESIAN_POINT('Ctrl Pts',(271.285463185231,90.9571441468218,274.905982351229));
#20762=CARTESIAN_POINT('Ctrl Pts',(270.847729939072,90.7494407701335,273.733052553961));
#20763=CARTESIAN_POINT('Ctrl Pts',(270.187343357388,91.7030860232968,273.222894193987));
#20764=CARTESIAN_POINT('Ctrl Pts',(270.946701599761,90.7857513677001,275.057147077298));
#20765=CARTESIAN_POINT('Ctrl Pts',(270.548229297884,90.5841485940949,273.76942958616));
#20766=CARTESIAN_POINT('Ctrl Pts',(269.82981977108,91.6423159687712,273.29846276181));
#20767=CARTESIAN_POINT('Origin',(273.70485351704,93.8763964470762,271.539778446323));
#20768=CARTESIAN_POINT('Origin',(289.522998818702,72.7829756068832,232.288983442877));
#20769=CARTESIAN_POINT('Origin',(259.80186267196,79.6360819935406,232.288983442877));
#20770=CARTESIAN_POINT('Origin',(273.70485351704,93.8763964470762,225.073593133703));
#20771=CARTESIAN_POINT('Origin',(273.70485351704,93.8763964470762,234.607407821084));
#20772=CARTESIAN_POINT('Origin',(292.443899216281,85.4505855182842,234.607407821084));
#20773=CARTESIAN_POINT('Ctrl Pts',(269.82981977108,91.6423159687712,232.848723505596));
#20774=CARTESIAN_POINT('Ctrl Pts',(270.015561437251,91.6738873996182,232.887983101985));
#20775=CARTESIAN_POINT('Ctrl Pts',(270.200459723154,91.7023018694398,232.93115673308));
#20776=CARTESIAN_POINT('Ctrl Pts',(270.384451598149,91.7278499278192,232.978338693559));
#20777=CARTESIAN_POINT('Ctrl Pts',(270.521635861377,91.7468985492097,233.013517543094));
#20778=CARTESIAN_POINT('Ctrl Pts',(270.65831599323,91.7643530228057,233.050925525407));
#20779=CARTESIAN_POINT('Ctrl Pts',(270.794458168282,91.7803254248894,233.090616791577));
#20780=CARTESIAN_POINT('Ctrl Pts',(270.827503889548,91.7842023979656,233.100251032532));
#20781=CARTESIAN_POINT('Ctrl Pts',(270.860514172686,91.7879920027267,233.110019115394));
#20782=CARTESIAN_POINT('Ctrl Pts',(270.893491220388,91.7916960151221,233.119922617088));
#20783=CARTESIAN_POINT('Ctrl Pts',(271.019946239265,91.8058995594058,233.157898954599));
#20784=CARTESIAN_POINT('Ctrl Pts',(271.145979477639,91.818840099349,233.197817538844));
#20785=CARTESIAN_POINT('Ctrl Pts',(271.271436525776,91.8305893739001,233.240086590348));
#20786=CARTESIAN_POINT('Ctrl Pts',(271.387350430509,91.8414449161849,233.279140361196));
#20787=CARTESIAN_POINT('Ctrl Pts',(271.502772822986,91.8512832807417,233.320200439574));
#20788=CARTESIAN_POINT('Ctrl Pts',(271.617555868356,91.860152164324,233.363624493924));
#20789=CARTESIAN_POINT('Ctrl Pts',(271.658627289105,91.8633256090432,233.379162395023));
#20790=CARTESIAN_POINT('Ctrl Pts',(271.69961657089,91.8663748568654,233.395003328621));
#20791=CARTESIAN_POINT('Ctrl Pts',(271.740515912666,91.8693018708402,233.411164981821));
#20792=CARTESIAN_POINT('Ctrl Pts',(271.799838261565,91.8735473510047,233.434606611642));
#20793=CARTESIAN_POINT('Ctrl Pts',(271.858885216673,91.8775346062734,233.458693452383));
#20794=CARTESIAN_POINT('Ctrl Pts',(271.917789704208,91.8812783618145,233.483545832084));
#20795=CARTESIAN_POINT('Ctrl Pts',(271.98067891853,91.8852753721348,233.510079407009));
#20796=CARTESIAN_POINT('Ctrl Pts',(272.043187679696,91.8889798656512,233.537425061905));
#20797=CARTESIAN_POINT('Ctrl Pts',(272.105263898368,91.8924068510043,233.565755425312));
#20798=CARTESIAN_POINT('Ctrl Pts',(272.162046353164,91.8955415883492,233.591669819165));
#20799=CARTESIAN_POINT('Ctrl Pts',(272.218467233987,91.8984440130497,233.618408205897));
#20800=CARTESIAN_POINT('Ctrl Pts',(272.274449019999,91.9011207122047,233.646122140915));
#20801=CARTESIAN_POINT('Ctrl Pts',(272.315013893718,91.9030602709602,233.666203891684));
#20802=CARTESIAN_POINT('Ctrl Pts',(272.355347522225,91.9048812121483,233.686798232757));
#20803=CARTESIAN_POINT('Ctrl Pts',(272.395404653415,91.9065846709651,233.707969914034));
#20804=CARTESIAN_POINT('Ctrl Pts',(272.439578572256,91.9084631991894,233.731317470453));
#20805=CARTESIAN_POINT('Ctrl Pts',(272.483534972761,91.9102014129653,233.755434280492));
#20806=CARTESIAN_POINT('Ctrl Pts',(272.527036273113,91.9118021664447,233.78039055539));
#20807=CARTESIAN_POINT('Ctrl Pts',(272.566794344995,91.9132651772372,233.80319937635));
#20808=CARTESIAN_POINT('Ctrl Pts',(272.60617228052,91.9146133414286,233.826709489539));
#20809=CARTESIAN_POINT('Ctrl Pts',(272.644950932319,91.9158481686079,233.850980212717));
#20810=CARTESIAN_POINT('Ctrl Pts',(272.677190170571,91.9168747614827,233.871158057762));
#20811=CARTESIAN_POINT('Ctrl Pts',(272.708956236063,91.9178216757778,233.891824193169));
#20812=CARTESIAN_POINT('Ctrl Pts',(272.740208285718,91.9186928087398,233.913085540272));
#20813=CARTESIAN_POINT('Ctrl Pts',(272.766064785827,91.9194135438524,233.930676195277));
#20814=CARTESIAN_POINT('Ctrl Pts',(272.791569024412,91.9200823513293,233.94867448331));
#20815=CARTESIAN_POINT('Ctrl Pts',(272.816671412602,91.9207001828372,233.967147124109));
#20816=CARTESIAN_POINT('Ctrl Pts',(272.843301300097,91.9213556098597,233.986743839071));
#20817=CARTESIAN_POINT('Ctrl Pts',(272.869552519657,91.9219560900281,234.006908595747));
#20818=CARTESIAN_POINT('Ctrl Pts',(272.895300543815,91.9225047161967,234.027756395878));
#20819=CARTESIAN_POINT('Ctrl Pts',(272.920502151311,91.9230416995891,234.048161770398));
#20820=CARTESIAN_POINT('Ctrl Pts',(272.945222322143,91.9235289788969,234.069221401029));
#20821=CARTESIAN_POINT('Ctrl Pts',(272.969294562453,91.9239691023271,234.091056293083));
#20822=CARTESIAN_POINT('Ctrl Pts',(272.991562003493,91.924376227813,234.111254129478));
#20823=CARTESIAN_POINT('Ctrl Pts',(273.013275095638,91.9247429811296,234.132115361817));
#20824=CARTESIAN_POINT('Ctrl Pts',(273.034255030787,91.9250714239154,234.153747492021));
#20825=CARTESIAN_POINT('Ctrl Pts',(273.035955476365,91.925098044545,234.155500798687));
#20826=CARTESIAN_POINT('Ctrl Pts',(273.037651077778,91.9251244136322,234.157259176335));
#20827=CARTESIAN_POINT('Ctrl Pts',(273.039341724696,91.9251505323558,234.159022685846));
#20828=CARTESIAN_POINT('Ctrl Pts',(273.058417945833,91.9254452399859,234.17892104371));
#20829=CARTESIAN_POINT('Ctrl Pts',(273.076927481094,91.9257089467546,234.199534667638));
#20830=CARTESIAN_POINT('Ctrl Pts',(273.094667580603,91.9259425960946,234.220959767754));
#20831=CARTESIAN_POINT('Ctrl Pts',(273.107225770739,91.9261079961159,234.236126564354));
#20832=CARTESIAN_POINT('Ctrl Pts',(273.11939749702,91.9262583450989,234.251700218268));
#20833=CARTESIAN_POINT('Ctrl Pts',(273.131095302992,91.9263942221247,234.267718436237));
#20834=CARTESIAN_POINT('Ctrl Pts',(273.146911991866,91.9265779424434,234.289376785718));
#20835=CARTESIAN_POINT('Ctrl Pts',(273.16170916562,91.9267367413741,234.31169009652));
#20836=CARTESIAN_POINT('Ctrl Pts',(273.175229567178,91.9268714448707,234.334711651649));
#20837=CARTESIAN_POINT('Ctrl Pts',(273.180570546791,91.9269246569463,234.343805882769));
#20838=CARTESIAN_POINT('Ctrl Pts',(273.185711732346,91.9269741156589,234.353010655731));
#20839=CARTESIAN_POINT('Ctrl Pts',(273.190634985725,91.9270199005296,234.362329333268));
#20840=CARTESIAN_POINT('Ctrl Pts',(273.200954484681,91.9271158689653,234.381861962547));
#20841=CARTESIAN_POINT('Ctrl Pts',(273.210366129408,91.9271982025984,234.402014498081));
#20842=CARTESIAN_POINT('Ctrl Pts',(273.218596491308,91.9272662961898,234.422661527238));
#20843=CARTESIAN_POINT('Ctrl Pts',(273.22647599308,91.9273314869531,234.442428374046));
#20844=CARTESIAN_POINT('Ctrl Pts',(273.233272329597,91.9273836561975,234.462648391072));
#20845=CARTESIAN_POINT('Ctrl Pts',(273.238790086692,91.9274236510184,234.483204447906));
#20846=CARTESIAN_POINT('Ctrl Pts',(273.244214637016,91.9274629702408,234.503413268778));
#20847=CARTESIAN_POINT('Ctrl Pts',(273.248402941013,91.92749054973,234.523946829525));
#20848=CARTESIAN_POINT('Ctrl Pts',(273.251220475383,91.9275081462254,234.544687559797));
#20849=CARTESIAN_POINT('Ctrl Pts',(273.254038009754,91.9275257427209,234.56542829007));
#20850=CARTESIAN_POINT('Ctrl Pts',(273.255484226474,91.927533383468,234.586376152881));
#20851=CARTESIAN_POINT('Ctrl Pts',(273.255484225105,91.9275333837837,234.607407821084));
#20852=CARTESIAN_POINT('Ctrl Pts',(259.737667058827,79.3576729844988,230.309496805655));
#20853=CARTESIAN_POINT('Ctrl Pts',(259.352493380025,77.6872189302482,230.556932635308));
#20854=CARTESIAN_POINT('Ctrl Pts',(259.352493380025,77.6872189302482,232.288983442877));
#20855=CARTESIAN_POINT('Ctrl Pts',(260.489866638734,79.1842306313197,230.309496805879));
#20856=CARTESIAN_POINT('Ctrl Pts',(259.96963870844,77.5449174176977,230.556932635576));
#20857=CARTESIAN_POINT('Ctrl Pts',(259.950395610518,77.5493544968644,232.288983443048));
#20858=CARTESIAN_POINT('Ctrl Pts',(261.204913401151,78.9177192700331,230.32315997602));
#20859=CARTESIAN_POINT('Ctrl Pts',(260.556326304222,77.3317737998227,230.575081299956));
#20860=CARTESIAN_POINT('Ctrl Pts',(260.520304163103,77.3441824757216,232.301458511035));
#20861=CARTESIAN_POINT('Ctrl Pts',(262.223292632623,78.383567916756,230.369110269103));
#20862=CARTESIAN_POINT('Ctrl Pts',(261.399847181909,76.9039004839053,230.632620004888));
#20863=CARTESIAN_POINT('Ctrl Pts',(261.334314889639,76.9392458488658,232.343413127113));
#20864=CARTESIAN_POINT('Ctrl Pts',(262.555366780788,78.1816425648538,230.38896060812));
#20865=CARTESIAN_POINT('Ctrl Pts',(261.6753798258,76.742552789912,230.657062473388));
#20866=CARTESIAN_POINT('Ctrl Pts',(261.600168265845,76.7869681618154,232.361537349181));
#20867=CARTESIAN_POINT('Ctrl Pts',(263.192272886508,77.7364025768308,230.439567449033));
#20868=CARTESIAN_POINT('Ctrl Pts',(262.205789159917,76.3857612367115,230.717576280988));
#20869=CARTESIAN_POINT('Ctrl Pts',(262.110942369255,76.4526422432372,232.407743595821));
#20870=CARTESIAN_POINT('Ctrl Pts',(263.494777280234,77.4950731950091,230.470081140236));
#20871=CARTESIAN_POINT('Ctrl Pts',(262.458640311379,76.1920833314033,230.753306404236));
#20872=CARTESIAN_POINT('Ctrl Pts',(262.353991061074,76.2720769658325,232.435603921899));
#20873=CARTESIAN_POINT('Ctrl Pts',(264.068873292152,76.9765864414354,230.544184477118));
#20874=CARTESIAN_POINT('Ctrl Pts',(262.93982714268,75.7742357891063,230.837564148899));
#20875=CARTESIAN_POINT('Ctrl Pts',(262.816166800432,75.8852869421232,232.503263491111));
#20876=CARTESIAN_POINT('Ctrl Pts',(264.340460862299,76.6994232039253,230.587767815121));
#20877=CARTESIAN_POINT('Ctrl Pts',(263.168240525539,75.5501498442423,230.886047592305));
#20878=CARTESIAN_POINT('Ctrl Pts',(263.035290733391,75.6790579795884,232.543056972796));
#20879=CARTESIAN_POINT('Ctrl Pts',(264.852462244799,76.109492954915,230.691718673468));
#20880=CARTESIAN_POINT('Ctrl Pts',(263.599273270706,75.0709585050467,230.998556574986));
#20881=CARTESIAN_POINT('Ctrl Pts',(263.449407025873,75.2411080436715,232.637968626996));
#20882=CARTESIAN_POINT('Ctrl Pts',(265.094373229635,75.7942915062606,230.752634143475));
#20883=CARTESIAN_POINT('Ctrl Pts',(263.803351197743,74.8137915708696,231.063135696844));
#20884=CARTESIAN_POINT('Ctrl Pts',(263.645621061591,75.0075891196608,232.693587098739));
#20885=CARTESIAN_POINT('Ctrl Pts',(265.756639414064,74.8164649195093,230.963024899036));
#20886=CARTESIAN_POINT('Ctrl Pts',(264.360159533119,74.0132571206067,231.280658468406));
#20887=CARTESIAN_POINT('Ctrl Pts',(264.18452429865,74.2844949805711,232.885683007215));
#20888=CARTESIAN_POINT('Ctrl Pts',(266.116520847411,74.1216801997293,231.139458375964));
#20889=CARTESIAN_POINT('Ctrl Pts',(264.662785788949,73.4369654879794,231.457867253309));
#20890=CARTESIAN_POINT('Ctrl Pts',(264.479839828954,73.7723884511474,233.046772261445));
#20891=CARTESIAN_POINT('Ctrl Pts',(266.39885077907,73.3906559987533,231.366755111123));
#20892=CARTESIAN_POINT('Ctrl Pts',(264.891797790303,72.8283445041923,231.677295442204));
#20893=CARTESIAN_POINT('Ctrl Pts',(264.714335805196,73.2350168556771,233.254306243521));
#20894=CARTESIAN_POINT('Ctrl Pts',(264.697446445794,73.2734364402351,233.239531476064));
#20895=CARTESIAN_POINT('Ctrl Pts',(264.654229186946,73.3710281088638,233.167817844006));
#20896=CARTESIAN_POINT('Ctrl Pts',(264.609313044049,73.4689055458569,233.096787663571));
#20897=CARTESIAN_POINT('Ctrl Pts',(264.562879524106,73.5667785698821,233.026632701688));
#20898=CARTESIAN_POINT('Ctrl Pts',(264.516195848542,73.665178874352,232.956099787454));
#20899=CARTESIAN_POINT('Ctrl Pts',(264.467978434442,73.7635743807309,232.88645157777));
#20900=CARTESIAN_POINT('Ctrl Pts',(264.418450588595,73.8616684422313,232.817847262986));
#20901=CARTESIAN_POINT('Ctrl Pts',(264.40679314368,73.884756991691,232.801699760366));
#20902=CARTESIAN_POINT('Ctrl Pts',(264.395063267842,73.9078288468005,232.78560993391));
#20903=CARTESIAN_POINT('Ctrl Pts',(264.383264177312,73.9308801593125,232.769579574183));
#20904=CARTESIAN_POINT('Ctrl Pts',(264.313305252971,74.0675555262783,232.674532695741));
#20905=CARTESIAN_POINT('Ctrl Pts',(264.240690520829,74.2039410093792,232.581287471137));
#20906=CARTESIAN_POINT('Ctrl Pts',(264.165615557534,74.3400654072201,232.489700248591));
#20907=CARTESIAN_POINT('Ctrl Pts',(264.120725662995,74.4214588517848,232.434937108116));
#20908=CARTESIAN_POINT('Ctrl Pts',(264.074956495285,74.5027582590142,232.380767208533));
#20909=CARTESIAN_POINT('Ctrl Pts',(264.028354597553,74.5839630677654,232.327163638241));
#20910=CARTESIAN_POINT('Ctrl Pts',(263.985456304859,74.6587142651096,232.277820118777));
#20911=CARTESIAN_POINT('Ctrl Pts',(263.941868682874,74.7333559521437,232.228977938585));
#20912=CARTESIAN_POINT('Ctrl Pts',(263.897622680722,74.8078999837302,232.180607335982));
#20913=CARTESIAN_POINT('Ctrl Pts',(263.825507862472,74.9293963682165,232.101769993722));
#20914=CARTESIAN_POINT('Ctrl Pts',(263.751669999091,75.0506924616519,232.024180793303));
#20915=CARTESIAN_POINT('Ctrl Pts',(263.676293153804,75.1720265572414,231.947761794839));
#20916=CARTESIAN_POINT('Ctrl Pts',(263.603251188336,75.2896021971659,231.873709958022));
#20917=CARTESIAN_POINT('Ctrl Pts',(263.528763284777,75.4072132185362,231.800757130054));
#20918=CARTESIAN_POINT('Ctrl Pts',(263.453038257345,75.5250695290885,231.728853068671));
#20919=CARTESIAN_POINT('Ctrl Pts',(263.394019028683,75.6169254026021,231.672811857669));
#20920=CARTESIAN_POINT('Ctrl Pts',(263.334291283429,75.7088649691641,231.617453519133));
#20921=CARTESIAN_POINT('Ctrl Pts',(263.274112511905,75.8008447270264,231.562900942566));
#20922=CARTESIAN_POINT('Ctrl Pts',(263.256213869813,75.8282017621411,231.546675668795));
#20923=CARTESIAN_POINT('Ctrl Pts',(263.238275603622,75.8555622284378,231.530521839858));
#20924=CARTESIAN_POINT('Ctrl Pts',(263.22030522037,75.8829246557764,231.51444312478));
#20925=CARTESIAN_POINT('Ctrl Pts',(263.165709508658,75.9660542793201,231.465594478605));
#20926=CARTESIAN_POINT('Ctrl Pts',(263.110705657456,76.0493669964364,231.417342430414));
#20927=CARTESIAN_POINT('Ctrl Pts',(263.055520334322,76.1328170019997,231.369809600742));
#20928=CARTESIAN_POINT('Ctrl Pts',(263.038785104679,76.158123640205,231.355395028625));
#20929=CARTESIAN_POINT('Ctrl Pts',(263.022033475043,76.1834427777927,231.341046764967));
#20930=CARTESIAN_POINT('Ctrl Pts',(263.005272555421,76.2087727973911,231.326768677458));
#20931=CARTESIAN_POINT('Ctrl Pts',(262.947061992686,76.2967437875341,231.277180974194));
#20932=CARTESIAN_POINT('Ctrl Pts',(262.888651064932,76.384974810687,231.228304565985));
#20933=CARTESIAN_POINT('Ctrl Pts',(262.830207117975,76.4736562503305,231.180271844975));
#20934=CARTESIAN_POINT('Ctrl Pts',(262.773496656583,76.5597073406654,231.133663805781));
#20935=CARTESIAN_POINT('Ctrl Pts',(262.716754900792,76.646182300906,231.087850087869));
#20936=CARTESIAN_POINT('Ctrl Pts',(262.660170090237,76.7332741961984,231.042976730252));
#20937=CARTESIAN_POINT('Ctrl Pts',(262.606111579047,76.8164777653204,231.000106799592));
#20938=CARTESIAN_POINT('Ctrl Pts',(262.552196231045,76.9002442747484,230.958095150216));
#20939=CARTESIAN_POINT('Ctrl Pts',(262.498622814573,76.9847622690485,230.917092579518));
#20940=CARTESIAN_POINT('Ctrl Pts',(262.451137883189,77.0596750042147,230.880749848657));
#20941=CARTESIAN_POINT('Ctrl Pts',(262.403921887061,77.1351782564116,230.845200112458));
#20942=CARTESIAN_POINT('Ctrl Pts',(262.357138788268,77.2114190794966,230.810565027849));
#20943=CARTESIAN_POINT('Ctrl Pts',(262.31561657369,77.2790864187155,230.779824750864));
#20944=CARTESIAN_POINT('Ctrl Pts',(262.274464121646,77.3472811150659,230.749829012529));
#20945=CARTESIAN_POINT('Ctrl Pts',(262.233715133929,77.4162867755718,230.720601932399));
#20946=CARTESIAN_POINT('Ctrl Pts',(262.219591643633,77.4402039531783,230.710471904496));
#20947=CARTESIAN_POINT('Ctrl Pts',(262.205516943508,77.4642186345719,230.700434512941));
#20948=CARTESIAN_POINT('Ctrl Pts',(262.191493523411,77.4883429401725,230.690491742317));
#20949=CARTESIAN_POINT('Ctrl Pts',(262.153645195841,77.5534529215029,230.663656830653));
#20950=CARTESIAN_POINT('Ctrl Pts',(262.116452720228,77.6188974008809,230.637693868061));
#20951=CARTESIAN_POINT('Ctrl Pts',(262.079950203966,77.6848975804388,230.612712308445));
#20952=CARTESIAN_POINT('Ctrl Pts',(262.044800464362,77.7484518052682,230.588656560914));
#20953=CARTESIAN_POINT('Ctrl Pts',(262.010290480822,77.8125210117592,230.565510694921));
#20954=CARTESIAN_POINT('Ctrl Pts',(261.976479795831,77.8773102687136,230.543410702692));
#20955=CARTESIAN_POINT('Ctrl Pts',(261.968393922972,77.8928047106185,230.538125458474));
#20956=CARTESIAN_POINT('Ctrl Pts',(261.960348181157,77.9083403809965,230.532900214237));
#20957=CARTESIAN_POINT('Ctrl Pts',(261.952343646247,77.9239201814014,230.527737185114));
#20958=CARTESIAN_POINT('Ctrl Pts',(261.915421006234,77.9957853638597,230.503921602098));
#20959=CARTESIAN_POINT('Ctrl Pts',(261.879415499712,78.0685007726458,230.48145621462));
#20960=CARTESIAN_POINT('Ctrl Pts',(261.844512219108,78.1422191631716,230.460620223486));
#20961=CARTESIAN_POINT('Ctrl Pts',(261.810342116173,78.2143890265434,230.440221912798));
#20962=CARTESIAN_POINT('Ctrl Pts',(261.777228382095,78.2875199945043,230.421385152265));
#20963=CARTESIAN_POINT('Ctrl Pts',(261.745364910435,78.3617834768448,230.404406843503));
#20964=CARTESIAN_POINT('Ctrl Pts',(261.714466316366,78.4337981405152,230.387942665463));
#20965=CARTESIAN_POINT('Ctrl Pts',(261.684743410344,78.506877645955,230.373226044139));
#20966=CARTESIAN_POINT('Ctrl Pts',(261.656392439806,78.5812071226677,230.360561957802));
#20967=CARTESIAN_POINT('Ctrl Pts',(261.641714198808,78.6196899665266,230.35400533883));
#20968=CARTESIAN_POINT('Ctrl Pts',(261.627404024125,78.658508350682,230.347999468436));
#20969=CARTESIAN_POINT('Ctrl Pts',(261.613491303169,78.6976913251228,230.342590522453));
#20970=CARTESIAN_POINT('Ctrl Pts',(270.946701599761,90.7857513677001,231.090039190109));
#20971=CARTESIAN_POINT('Ctrl Pts',(270.548229297884,90.584148594095,232.377756681246));
#20972=CARTESIAN_POINT('Ctrl Pts',(269.82981977108,91.6423159687712,232.848723505596));
#20973=CARTESIAN_POINT('Ctrl Pts',(271.286862403972,90.9578520664885,231.241828286301));
#20974=CARTESIAN_POINT('Ctrl Pts',(270.848946691457,90.7501122866934,232.414281499181));
#20975=CARTESIAN_POINT('Ctrl Pts',(270.188821842695,91.7033373287686,232.924604575929));
#20976=CARTESIAN_POINT('Ctrl Pts',(271.6212194979,91.1089748570485,231.422589429823));
#20977=CARTESIAN_POINT('Ctrl Pts',(271.165120845064,90.9088548773701,232.486141144197));
#20978=CARTESIAN_POINT('Ctrl Pts',(270.544092776974,91.752458983209,233.01499862562));
#20979=CARTESIAN_POINT('Ctrl Pts',(272.275527462515,91.375506398507,231.842314946566));
#20980=CARTESIAN_POINT('Ctrl Pts',(271.798039921684,91.1948055159721,232.698358378032));
#20981=CARTESIAN_POINT('Ctrl Pts',(271.24287296878,91.830953766497,233.224861383659));
#20982=CARTESIAN_POINT('Ctrl Pts',(272.595862729514,91.4909084601913,232.080552096927));
#20983=CARTESIAN_POINT('Ctrl Pts',(272.117008863945,91.3240589446257,232.836133673852));
#20984=CARTESIAN_POINT('Ctrl Pts',(271.586877031609,91.8602853819312,233.343979959847));
#20985=CARTESIAN_POINT('Ctrl Pts',(273.055973002656,91.6390983881989,232.499348715414));
#20986=CARTESIAN_POINT('Ctrl Pts',(272.583967923736,91.4932491614987,233.105225965723));
#20987=CARTESIAN_POINT('Ctrl Pts',(272.083191646016,91.891821899915,233.553378267828));
#20988=CARTESIAN_POINT('Ctrl Pts',(273.204529404127,91.6838758628784,232.648354966299));
#20989=CARTESIAN_POINT('Ctrl Pts',(272.735069316385,91.5447528864996,233.203629145364));
#20990=CARTESIAN_POINT('Ctrl Pts',(272.243823100579,91.9001534779783,233.627881394136));
#20991=CARTESIAN_POINT('Ctrl Pts',(273.484341261294,91.7635443402254,232.968742094674));
#20992=CARTESIAN_POINT('Ctrl Pts',(273.020860725553,91.6369710951425,233.421501455589));
#20993=CARTESIAN_POINT('Ctrl Pts',(272.546965968386,91.9130290682149,233.788074957434));
#20994=CARTESIAN_POINT('Ctrl Pts',(273.616857737478,91.7987484382474,233.141703545685));
#20995=CARTESIAN_POINT('Ctrl Pts',(273.15739221448,91.6782943342807,233.542090459735));
#20996=CARTESIAN_POINT('Ctrl Pts',(272.690849322385,91.9176033917613,233.874555683821));
#20997=CARTESIAN_POINT('Ctrl Pts',(273.848277352538,91.8572508300294,233.512069308584));
#20998=CARTESIAN_POINT('Ctrl Pts',(273.396194529834,91.7472262082025,233.805283770732));
#20999=CARTESIAN_POINT('Ctrl Pts',(272.942493502819,91.9237969739132,234.059738564397));
#21000=CARTESIAN_POINT('Ctrl Pts',(273.948668648815,91.8809506992841,233.711024516524));
#21001=CARTESIAN_POINT('Ctrl Pts',(273.500654142745,91.77553083905,233.949189921464));
#21002=CARTESIAN_POINT('Ctrl Pts',(273.051869353513,91.9254713513345,234.159216168977));
#21003=CARTESIAN_POINT('Ctrl Pts',(274.09398531746,91.9143029740673,234.145040928275));
#21004=CARTESIAN_POINT('Ctrl Pts',(273.651605727385,91.8153497331837,234.266111504467));
#21005=CARTESIAN_POINT('Ctrl Pts',(273.210311012066,91.9273201034252,234.376224374506));
#21006=CARTESIAN_POINT('Ctrl Pts',(274.135356638104,91.9232791790263,234.372165957108));
#21007=CARTESIAN_POINT('Ctrl Pts',(273.694940786991,91.8262033927225,234.433947592198));
#21008=CARTESIAN_POINT('Ctrl Pts',(273.255484232762,91.9275333820181,234.489786889222));
#21009=CARTESIAN_POINT('Ctrl Pts',(274.135356630693,91.9232791773928,234.607407821084));
#21010=CARTESIAN_POINT('Ctrl Pts',(273.694940779299,91.8262033907668,234.607407821084));
#21011=CARTESIAN_POINT('Ctrl Pts',(273.255484225105,91.9275333837837,234.607407821084));
#21012=CARTESIAN_POINT('Origin',(270.043805148192,92.5703459989105,231.090039190109));
#21013=CARTESIAN_POINT('Ctrl Pts',(261.613491303076,78.6976913253861,230.342590522417));
#21014=CARTESIAN_POINT('Ctrl Pts',(263.538250261041,78.7291375341272,230.271134115559));
#21015=CARTESIAN_POINT('Ctrl Pts',(263.544486310321,78.4442745295379,228.365981599697));
#21016=CARTESIAN_POINT('Ctrl Pts',(261.754727069591,78.2999231643027,230.397499740681));
#21017=CARTESIAN_POINT('Ctrl Pts',(263.533654545715,78.3947691062589,230.197080913061));
#21018=CARTESIAN_POINT('Ctrl Pts',(263.557302515181,77.8588297294342,228.466535359745));
#21019=CARTESIAN_POINT('Ctrl Pts',(261.949245797898,77.905077339807,230.518734113756));
#21020=CARTESIAN_POINT('Ctrl Pts',(263.538547887166,77.9742246260869,230.184893838673));
#21021=CARTESIAN_POINT('Ctrl Pts',(263.606591880382,77.3148820941748,228.695704330778));
#21022=CARTESIAN_POINT('Ctrl Pts',(262.433710331117,77.0716088320361,230.862258230087));
#21023=CARTESIAN_POINT('Ctrl Pts',(263.62457185023,77.0153725192018,230.390094211506));
#21024=CARTESIAN_POINT('Ctrl Pts',(263.755975405511,76.2858158960459,229.333149475148));
#21025=CARTESIAN_POINT('Ctrl Pts',(262.711999049712,76.651982580077,231.07693973435));
#21026=CARTESIAN_POINT('Ctrl Pts',(263.698661733633,76.5115820479241,230.587426418292));
#21027=CARTESIAN_POINT('Ctrl Pts',(263.852404590493,75.8249982256616,229.727424668816));
#21028=CARTESIAN_POINT('Ctrl Pts',(263.151909041546,75.9871679741599,231.451683298859));
#21029=CARTESIAN_POINT('Ctrl Pts',(263.858168373587,75.7622723596515,231.014329531148));
#21030=CARTESIAN_POINT('Ctrl Pts',(264.014706007827,75.1891126872917,230.390979291267));
#21031=CARTESIAN_POINT('Ctrl Pts',(263.302835955366,75.7588393827039,231.586229920659));
#21032=CARTESIAN_POINT('Ctrl Pts',(263.917768744924,75.5167006386232,231.174220647959));
#21033=CARTESIAN_POINT('Ctrl Pts',(264.072112191274,74.9857513363428,230.625585659508));
#21034=CARTESIAN_POINT('Ctrl Pts',(263.603229270728,75.2913050055119,231.871484249179));
#21035=CARTESIAN_POINT('Ctrl Pts',(264.048271575524,75.0381564136451,231.523754885091));
#21036=CARTESIAN_POINT('Ctrl Pts',(264.190557682095,74.5984025565875,231.111812803299));
#21037=CARTESIAN_POINT('Ctrl Pts',(263.752412397553,75.0525305312736,232.021888703375));
#21038=CARTESIAN_POINT('Ctrl Pts',(264.119123197883,74.8037832321443,231.713284495735));
#21039=CARTESIAN_POINT('Ctrl Pts',(264.251478238827,74.4146529473821,231.362943463785));
#21040=CARTESIAN_POINT('Ctrl Pts',(264.18801223314,74.318663255928,232.498072233561));
#21041=CARTESIAN_POINT('Ctrl Pts',(264.343108315152,74.1265992211969,232.310088246099));
#21042=CARTESIAN_POINT('Ctrl Pts',(264.437749904701,73.8878858377892,232.136325187552));
#21043=CARTESIAN_POINT('Ctrl Pts',(264.462022086343,73.805063319091,232.848874208672));
#21044=CARTESIAN_POINT('Ctrl Pts',(264.514363032579,73.6868688639842,232.764079118951));
#21045=CARTESIAN_POINT('Ctrl Pts',(264.566427694476,73.5692983043056,232.678673032712));
#21046=CARTESIAN_POINT('Ctrl Pts',(264.697446473732,73.2734363771458,233.239531522425));
#21047=CARTESIAN_POINT('Ctrl Pts',(264.697446473732,73.2734363771458,233.239531522425));
#21048=CARTESIAN_POINT('Ctrl Pts',(264.697446473732,73.2734363771458,233.239531522425));
#21049=CARTESIAN_POINT('Origin',(261.544965371427,78.4005022217613,228.365981599697));
#21050=CARTESIAN_POINT('Ctrl Pts',(269.854275011351,91.6534391605604,232.857577006965));
#21051=CARTESIAN_POINT('Ctrl Pts',(270.570059236857,90.5960147688002,232.385774045372));
#21052=CARTESIAN_POINT('Ctrl Pts',(270.968300873754,90.7966556084582,231.099602120239));
#21053=CARTESIAN_POINT('Ctrl Pts',(268.604744603454,91.0863950856132,232.405463537209));
#21054=CARTESIAN_POINT('Ctrl Pts',(269.432630245025,89.9764222651554,231.966890092694));
#21055=CARTESIAN_POINT('Ctrl Pts',(269.865690073407,90.2412177466641,230.608113673404));
#21056=CARTESIAN_POINT('Ctrl Pts',(267.464189276692,90.3711900279631,231.954019100255));
#21057=CARTESIAN_POINT('Ctrl Pts',(268.441024770316,89.2277365749088,231.570841083931));
#21058=CARTESIAN_POINT('Ctrl Pts',(268.856210587267,89.5480198264324,230.117467754446));
#21059=CARTESIAN_POINT('Ctrl Pts',(266.167696989619,89.2769186281834,231.44356147555));
#21060=CARTESIAN_POINT('Ctrl Pts',(267.355974305096,88.1615081899221,231.147215204369));
#21061=CARTESIAN_POINT('Ctrl Pts',(267.70390220799,88.49475462708,229.56261847886));
#21062=CARTESIAN_POINT('Ctrl Pts',(265.916094587479,89.0487894564945,231.344572511768));
#21063=CARTESIAN_POINT('Ctrl Pts',(267.143553518795,87.9376690682908,231.064711755392));
#21064=CARTESIAN_POINT('Ctrl Pts',(267.480019289714,88.2754841698382,229.45502105674));
#21065=CARTESIAN_POINT('Ctrl Pts',(265.4323791966,88.5772761662469,231.155524737661));
#21066=CARTESIAN_POINT('Ctrl Pts',(266.737690630021,87.4799990631403,230.908816464417));
#21067=CARTESIAN_POINT('Ctrl Pts',(267.049049592436,87.8228826485866,229.249532939607));
#21068=CARTESIAN_POINT('Ctrl Pts',(265.199425076782,88.3332231180283,231.065132840242));
#21069=CARTESIAN_POINT('Ctrl Pts',(266.543832749098,87.2455062460305,230.835276501227));
#21070=CARTESIAN_POINT('Ctrl Pts',(266.841215893656,87.588906918953,229.151280183409));
#21071=CARTESIAN_POINT('Ctrl Pts',(264.751404757504,87.8281195778466,230.893641171869));
#21072=CARTESIAN_POINT('Ctrl Pts',(266.173128968869,86.765355814543,230.697233263588));
#21073=CARTESIAN_POINT('Ctrl Pts',(266.440914797084,87.1052253190934,228.964874858366));
#21074=CARTESIAN_POINT('Ctrl Pts',(264.53633792299,87.5670701460064,230.812539697383));
#21075=CARTESIAN_POINT('Ctrl Pts',(265.99661567878,86.5197889764757,230.63287950567));
#21076=CARTESIAN_POINT('Ctrl Pts',(266.248446847576,86.8555204360023,228.876720429038));
#21077=CARTESIAN_POINT('Ctrl Pts',(264.124514799001,87.0272818564076,230.660721835472));
#21078=CARTESIAN_POINT('Ctrl Pts',(265.66024065455,86.0173256302242,230.513656268916));
#21079=CARTESIAN_POINT('Ctrl Pts',(265.879235516166,86.3397350702421,228.711699775841));
#21080=CARTESIAN_POINT('Ctrl Pts',(263.927191920059,86.7475695814584,230.58981851043));
#21081=CARTESIAN_POINT('Ctrl Pts',(265.500275599213,85.7597404016426,230.458803159134));
#21082=CARTESIAN_POINT('Ctrl Pts',(265.701980328563,86.0727273676906,228.634630347835));
#21083=CARTESIAN_POINT('Ctrl Pts',(263.371013260911,85.8919630165414,230.396915586166));
#21084=CARTESIAN_POINT('Ctrl Pts',(265.048852082573,84.9762036078638,230.310332484399));
#21085=CARTESIAN_POINT('Ctrl Pts',(265.201250579595,85.2567685807412,228.424951655098));
#21086=CARTESIAN_POINT('Ctrl Pts',(263.045775790527,85.2976453867214,230.293899870431));
#21087=CARTESIAN_POINT('Ctrl Pts',(264.789930470114,84.446363163279,230.234220035086));
#21088=CARTESIAN_POINT('Ctrl Pts',(264.906879405776,84.6910034207126,228.312977103783));
#21089=CARTESIAN_POINT('Ctrl Pts',(262.62687627125,84.3695387744554,230.181183241364));
#21090=CARTESIAN_POINT('Ctrl Pts',(264.453884252299,83.6314427756986,230.151510863018));
#21091=CARTESIAN_POINT('Ctrl Pts',(264.525038303666,83.808960737799,228.190457998417));
#21092=CARTESIAN_POINT('Ctrl Pts',(262.498781303485,84.0540433691424,230.150587542756));
#21093=CARTESIAN_POINT('Ctrl Pts',(264.35067673049,83.3559903592243,230.129269379279));
#21094=CARTESIAN_POINT('Ctrl Pts',(264.407749924432,83.5093611816478,228.157201521371));
#21095=CARTESIAN_POINT('Ctrl Pts',(262.26635036146,83.4103949526379,230.104064485338));
#21096=CARTESIAN_POINT('Ctrl Pts',(264.161522391596,82.7966223766408,230.095512210108));
#21097=CARTESIAN_POINT('Ctrl Pts',(264.193747582666,82.8986213128696,228.106632552918));
#21098=CARTESIAN_POINT('Ctrl Pts',(262.161617537659,83.0806079892046,230.088126104489));
#21099=CARTESIAN_POINT('Ctrl Pts',(264.075481010945,82.5118428801294,230.084054419952));
#21100=CARTESIAN_POINT('Ctrl Pts',(264.096659353448,82.5859337679919,228.089308076332));
#21101=CARTESIAN_POINT('Ctrl Pts',(261.888691546354,82.0869216485276,230.063791396278));
#21102=CARTESIAN_POINT('Ctrl Pts',(263.846724958899,81.6550061013845,230.066518035117));
#21103=CARTESIAN_POINT('Ctrl Pts',(263.841428021229,81.6444770955451,228.062857080858));
#21104=CARTESIAN_POINT('Ctrl Pts',(261.760569838213,81.4178671457201,230.078387323601));
#21105=CARTESIAN_POINT('Ctrl Pts',(263.733391992834,81.0841958360596,230.076835183321));
#21106=CARTESIAN_POINT('Ctrl Pts',(263.718253822345,81.0115115254556,228.078722362158));
#21107=CARTESIAN_POINT('Ctrl Pts',(261.60811471911,80.0651323652977,230.166713788174));
#21108=CARTESIAN_POINT('Ctrl Pts',(263.579114429171,79.9201348333107,230.140876788285));
#21109=CARTESIAN_POINT('Ctrl Pts',(263.562456729262,79.7335113896652,228.174730202189));
#21110=CARTESIAN_POINT('Ctrl Pts',(261.584153941217,79.3806125524342,230.240765568358));
#21111=CARTESIAN_POINT('Ctrl Pts',(263.538621025243,79.3309179399804,230.194359322608));
#21112=CARTESIAN_POINT('Ctrl Pts',(263.53014583648,79.0876936137149,228.255221557826));
#21113=CARTESIAN_POINT('Ctrl Pts',(261.613732932928,78.6920384763593,230.34343273927));
#21114=CARTESIAN_POINT('Ctrl Pts',(263.538324332359,78.7241922265802,230.271761815837));
#21115=CARTESIAN_POINT('Ctrl Pts',(263.544604216139,78.4389366559092,228.366817597905));
#21116=CARTESIAN_POINT('Origin',(126.004365242683,113.565857732007,235.454046952338));
#21117=CARTESIAN_POINT('Origin',(128.290003445999,123.478408390104,235.454046952333));
#21118=CARTESIAN_POINT('Origin',(123.718727039363,103.653307073912,235.454046952337));
#21119=CARTESIAN_POINT('Origin',(122.575907937704,98.6970317448653,244.263820043021));
#21120=CARTESIAN_POINT('Origin',(121.433088836045,93.7407564158189,253.073593133703));
#21121=CARTESIAN_POINT('Origin',(129.432822547662,128.434683719148,244.263820043021));
#21122=CARTESIAN_POINT('Origin',(130.575641649323,133.390959048194,253.073593133703));
#21123=CARTESIAN_POINT('Origin',(122.575907937704,98.6970317448653,261.883366224386));
#21124=CARTESIAN_POINT('Origin',(123.718727039364,103.653307073913,270.693139315068));
#21125=CARTESIAN_POINT('Origin',(129.432822547662,128.434683719148,261.883366224386));
#21126=CARTESIAN_POINT('Origin',(128.290003446003,123.4784083901,270.693139315068));
#21127=CARTESIAN_POINT('Origin',(126.004365242683,113.565857732007,270.693139315069));
#21128=CARTESIAN_POINT('Origin',(234.789304633949,166.98951318199,253.073593133703));
#21129=CARTESIAN_POINT('',(0.,0.,0.));
#21130=CARTESIAN_POINT('Origin',(35.8297426794921,134.358342876286,253.073593133703));
#21131=CARTESIAN_POINT('',(34.9033441517125,130.340658746376,266.452681293963));
#21132=CARTESIAN_POINT('',(34.9033441517133,130.340658746376,239.694504973444));
#21133=CARTESIAN_POINT('Origin',(35.8297426794921,134.358342876286,253.073593133703));
#21134=CARTESIAN_POINT('',(36.756141207271,138.376027006196,266.452681293963));
#21135=CARTESIAN_POINT('Ctrl Pts',(34.9033441517134,130.340658746376,266.452681293963));
#21136=CARTESIAN_POINT('Ctrl Pts',(34.7662765826152,130.87911435207,266.338527474787));
#21137=CARTESIAN_POINT('Ctrl Pts',(34.6744566711603,131.454679427698,266.253801129437));
#21138=CARTESIAN_POINT('Ctrl Pts',(34.5897191635504,132.90588139296,266.106625474983));
#21139=CARTESIAN_POINT('Ctrl Pts',(34.672455114567,133.79000188487,266.073593133703));
#21140=CARTESIAN_POINT('Ctrl Pts',(35.0381671811249,135.376053159637,266.073593133703));
#21141=CARTESIAN_POINT('Ctrl Pts',(35.3509231135055,136.207135591509,266.106625474983));
#21142=CARTESIAN_POINT('Ctrl Pts',(36.0625567285284,137.474710120736,266.253801129437));
#21143=CARTESIAN_POINT('Ctrl Pts',(36.3971341252449,137.951956407289,266.338527474787));
#21144=CARTESIAN_POINT('Ctrl Pts',(36.756141207271,138.376027006196,266.452681293963));
#21145=CARTESIAN_POINT('',(38.9753277230386,148.000384319333,253.073593133703));
#21146=CARTESIAN_POINT('Origin',(35.8297426794921,134.358342876286,253.073593133703));
#21147=CARTESIAN_POINT('',(36.5770953678107,146.500890547976,253.073593133703));
#21148=CARTESIAN_POINT('',(38.9753277230384,148.000384319333,253.073593133703));
#21149=CARTESIAN_POINT('Origin',(33.8808796161997,134.807712168221,253.073593133703));
#21150=CARTESIAN_POINT('',(36.7561412072705,138.376027006196,239.694504973443));
#21151=CARTESIAN_POINT('Origin',(35.8297426794921,134.358342876286,253.073593133703));
#21152=CARTESIAN_POINT('Ctrl Pts',(36.7561412072712,138.376027006196,239.694504973444));
#21153=CARTESIAN_POINT('Ctrl Pts',(36.397134125245,137.951956407289,239.808658792619));
#21154=CARTESIAN_POINT('Ctrl Pts',(36.0625567285284,137.474710120736,239.893385137969));
#21155=CARTESIAN_POINT('Ctrl Pts',(35.3509231135055,136.207135591509,240.040560792424));
#21156=CARTESIAN_POINT('Ctrl Pts',(35.0381671811249,135.376053159637,240.073593133703));
#21157=CARTESIAN_POINT('Ctrl Pts',(34.672455114567,133.79000188487,240.073593133703));
#21158=CARTESIAN_POINT('Ctrl Pts',(34.5897191635504,132.90588139296,240.040560792424));
#21159=CARTESIAN_POINT('Ctrl Pts',(34.6744566711603,131.454679427698,239.893385137969));
#21160=CARTESIAN_POINT('Ctrl Pts',(34.7662765826152,130.87911435207,239.808658792619));
#21161=CARTESIAN_POINT('Ctrl Pts',(34.9033441517133,130.340658746376,239.694504973444));
#21162=CARTESIAN_POINT('Origin',(43.625194932662,132.560865708545,228.073593133703));
#21163=CARTESIAN_POINT('',(52.3950787174781,130.538703894837,239.073593133703));
#21164=CARTESIAN_POINT('Ctrl Pts',(36.7561412072711,138.376027006196,239.694504973444));
#21165=CARTESIAN_POINT('Ctrl Pts',(37.3757148123747,139.107887080655,239.957180175221));
#21166=CARTESIAN_POINT('Ctrl Pts',(38.1032632208345,139.722699664096,240.284186300941));
#21167=CARTESIAN_POINT('Ctrl Pts',(39.7934459051052,140.779485676509,241.003527112932));
#21168=CARTESIAN_POINT('Ctrl Pts',(40.9089819966417,141.223731124707,241.45444414134));
#21169=CARTESIAN_POINT('Ctrl Pts',(43.2595652384548,141.632211467481,242.135542680051));
#21170=CARTESIAN_POINT('Ctrl Pts',(44.499373374861,141.595451762353,242.34978783894));
#21171=CARTESIAN_POINT('Ctrl Pts',(46.7953401178796,141.066047224369,242.34978783894));
#21172=CARTESIAN_POINT('Ctrl Pts',(47.9260656397772,140.556208735091,242.135542680051));
#21173=CARTESIAN_POINT('Ctrl Pts',(49.8604537880171,139.159698706815,241.45444414134));
#21174=CARTESIAN_POINT('Ctrl Pts',(50.6688322158806,138.271836607652,241.003527112932));
#21175=CARTESIAN_POINT('Ctrl Pts',(51.8384599473883,136.401179241243,240.207376376427));
#21176=CARTESIAN_POINT('Ctrl Pts',(52.2870155925865,135.282886966942,239.801293920092));
#21177=CARTESIAN_POINT('Ctrl Pts',(52.6974998422104,132.921179650313,239.231941806271));
#21178=CARTESIAN_POINT('Ctrl Pts',(52.6573682389623,131.676223457217,239.073593133703));
#21179=CARTESIAN_POINT('Ctrl Pts',(52.3950787174781,130.538703894837,239.073593133703));
#21180=CARTESIAN_POINT('',(52.3950787174781,130.538703894837,228.073593133703));
#21181=CARTESIAN_POINT('',(52.3950787174781,130.538703894837,228.073593133703));
#21182=CARTESIAN_POINT('Origin',(43.625194932662,132.560865708545,228.073593133703));
#21183=CARTESIAN_POINT('Ctrl Pts',(52.3950787174781,130.538703894837,239.073593133703));
#21184=CARTESIAN_POINT('Ctrl Pts',(52.1327891959939,129.401184332456,239.073593133703));
#21185=CARTESIAN_POINT('Ctrl Pts',(51.6237279274457,128.264354049093,239.231941806271));
#21186=CARTESIAN_POINT('Ctrl Pts',(50.2205453140278,126.32084245355,239.801293920092));
#21187=CARTESIAN_POINT('Ctrl Pts',(49.3276013266274,125.511873472089,240.207376376427));
#21188=CARTESIAN_POINT('Ctrl Pts',(47.4569439602189,124.342245740582,241.003527112932));
#21189=CARTESIAN_POINT('Ctrl Pts',(46.3414078686823,123.898000292383,241.45444414134));
#21190=CARTESIAN_POINT('Ctrl Pts',(43.9908246268693,123.489519949609,242.135542680051));
#21191=CARTESIAN_POINT('Ctrl Pts',(42.751016490463,123.526279654737,242.34978783894));
#21192=CARTESIAN_POINT('Ctrl Pts',(41.6030331189537,123.790981923729,242.34978783894));
#21193=CARTESIAN_POINT('Ctrl Pts',(40.4550497474444,124.055684192721,242.34978783894));
#21194=CARTESIAN_POINT('Ctrl Pts',(39.3243242255468,124.565522682,242.135542680051));
#21195=CARTESIAN_POINT('Ctrl Pts',(37.3899360773069,125.962032710275,241.45444414134));
#21196=CARTESIAN_POINT('Ctrl Pts',(36.5815576494434,126.849894809438,241.003527112932));
#21197=CARTESIAN_POINT('Ctrl Pts',(35.5247716370308,128.540077493709,240.284186300941));
#21198=CARTESIAN_POINT('Ctrl Pts',(35.1398950505134,129.411393287529,239.957180175221));
#21199=CARTESIAN_POINT('Ctrl Pts',(34.9033441517133,130.340658746376,239.694504973444));
#21200=CARTESIAN_POINT('Origin',(43.625194932662,132.560865708545,228.073593133703));
#21201=CARTESIAN_POINT('',(52.3950787174781,130.538703894837,278.073593133703));
#21202=CARTESIAN_POINT('Origin',(43.625194932662,132.560865708545,278.073593133703));
#21203=CARTESIAN_POINT('',(52.3950787174781,130.538703894837,267.073593133703));
#21204=CARTESIAN_POINT('',(52.3950787174781,130.538703894837,228.073593133703));
#21205=CARTESIAN_POINT('Ctrl Pts',(52.3950787174781,130.538703894837,267.073593133703));
#21206=CARTESIAN_POINT('Ctrl Pts',(52.6573682389623,131.676223457217,267.073593133703));
#21207=CARTESIAN_POINT('Ctrl Pts',(52.6974998422104,132.921179650313,266.915244461136));
#21208=CARTESIAN_POINT('Ctrl Pts',(52.2870155925865,135.282886966942,266.345892347314));
#21209=CARTESIAN_POINT('Ctrl Pts',(51.8384599473883,136.401179241243,265.939809890979));
#21210=CARTESIAN_POINT('Ctrl Pts',(50.6688322158806,138.271836607652,265.143659154474));
#21211=CARTESIAN_POINT('Ctrl Pts',(49.8604537880171,139.159698706815,264.692742126067));
#21212=CARTESIAN_POINT('Ctrl Pts',(47.9260656397772,140.556208735091,264.011643587355));
#21213=CARTESIAN_POINT('Ctrl Pts',(46.7953401178796,141.066047224369,263.797398428467));
#21214=CARTESIAN_POINT('Ctrl Pts',(44.499373374861,141.595451762353,263.797398428467));
#21215=CARTESIAN_POINT('Ctrl Pts',(43.2595652384548,141.632211467481,264.011643587355));
#21216=CARTESIAN_POINT('Ctrl Pts',(40.9089819966417,141.223731124707,264.692742126067));
#21217=CARTESIAN_POINT('Ctrl Pts',(39.7934459051052,140.779485676509,265.143659154474));
#21218=CARTESIAN_POINT('Ctrl Pts',(38.1032632208345,139.722699664096,265.862999966466));
#21219=CARTESIAN_POINT('Ctrl Pts',(37.3757148123746,139.107887080655,266.190006092186));
#21220=CARTESIAN_POINT('Ctrl Pts',(36.756141207271,138.376027006196,266.452681293963));
#21221=CARTESIAN_POINT('Ctrl Pts',(34.9033441517133,130.340658746376,266.452681293963));
#21222=CARTESIAN_POINT('Ctrl Pts',(35.1398950505135,129.411393287529,266.190006092186));
#21223=CARTESIAN_POINT('Ctrl Pts',(35.5247716370309,128.540077493709,265.862999966466));
#21224=CARTESIAN_POINT('Ctrl Pts',(36.5815576494434,126.849894809438,265.143659154474));
#21225=CARTESIAN_POINT('Ctrl Pts',(37.389936077307,125.962032710275,264.692742126067));
#21226=CARTESIAN_POINT('Ctrl Pts',(39.3243242255468,124.565522682,264.011643587355));
#21227=CARTESIAN_POINT('Ctrl Pts',(40.4550497474444,124.055684192721,263.797398428467));
#21228=CARTESIAN_POINT('Ctrl Pts',(41.6030331189537,123.790981923729,263.797398428467));
#21229=CARTESIAN_POINT('Ctrl Pts',(42.751016490463,123.526279654737,263.797398428467));
#21230=CARTESIAN_POINT('Ctrl Pts',(43.9908246268693,123.489519949609,264.011643587355));
#21231=CARTESIAN_POINT('Ctrl Pts',(46.3414078686823,123.898000292383,264.692742126067));
#21232=CARTESIAN_POINT('Ctrl Pts',(47.4569439602189,124.342245740582,265.143659154474));
#21233=CARTESIAN_POINT('Ctrl Pts',(49.3276013266274,125.511873472089,265.939809890979));
#21234=CARTESIAN_POINT('Ctrl Pts',(50.2205453140278,126.32084245355,266.345892347314));
#21235=CARTESIAN_POINT('Ctrl Pts',(51.6237279274458,128.264354049093,266.915244461136));
#21236=CARTESIAN_POINT('Ctrl Pts',(52.1327891959939,129.401184332456,267.073593133703));
#21237=CARTESIAN_POINT('Ctrl Pts',(52.3950787174781,130.538703894837,267.073593133703));
#21238=CARTESIAN_POINT('Origin',(75.0993334048352,125.303551643792,253.073593133703));
#21239=CARTESIAN_POINT('',(75.3216238534428,139.619647024742,253.073593133703));
#21240=CARTESIAN_POINT('',(69.0304537663503,112.335564138647,253.073593133703));
#21241=CARTESIAN_POINT('Origin',(72.1760388098966,125.977605581695,253.073593133703));
#21242=CARTESIAN_POINT('',(73.4141985600783,117.995315156445,253.073593133703));
#21243=CARTESIAN_POINT('',(73.4141985600783,117.995315156445,253.073593133703));
#21244=CARTESIAN_POINT('',(75.0993334048352,125.303551643792,245.573593133703));
#21245=CARTESIAN_POINT('Origin',(75.0993334048352,125.303551643792,253.073593133703));
#21246=CARTESIAN_POINT('Origin',(75.0993334048352,125.303551643792,253.073593133703));
#21247=CARTESIAN_POINT('Origin',(72.1760388098966,125.977605581695,253.073593133703));
#21248=CARTESIAN_POINT('Origin',(75.0993334048352,125.303551643792,253.073593133703));
#21249=CARTESIAN_POINT('',(201.775432518845,96.0945476680054,245.573593133703));
#21250=CARTESIAN_POINT('Origin',(201.775432518845,96.0945476680054,253.073593133703));
#21251=CARTESIAN_POINT('',(75.0993334048352,125.303551643792,245.573593133703));
#21252=CARTESIAN_POINT('Origin',(75.0993334048352,125.303551643792,253.073593133703));
#21253=CARTESIAN_POINT('',(78.2449184483815,138.945593086839,253.073593133703));
#21254=CARTESIAN_POINT('Origin',(201.775432518845,96.0945476680054,253.073593133703));
#21255=CARTESIAN_POINT('Origin',(33.8808796161997,134.807712168221,253.073593133703));
#21256=CARTESIAN_POINT('Origin',(43.625194932662,132.560865708545,278.073593133703));
#21257=CARTESIAN_POINT('Origin',(43.625194932662,132.560865708545,228.073593133703));
#21258=CARTESIAN_POINT('',(0.,0.,0.));
#21259=CARTESIAN_POINT('Origin',(271.986847992623,154.073622192239,260.573593133705));
#21260=CARTESIAN_POINT('',(268.41135366976,154.898060492931,258.981066262494));
#21261=CARTESIAN_POINT('Origin',(271.986847992623,154.073622192239,260.573593133705));
#21262=CARTESIAN_POINT('',(267.624957408873,151.487550132169,258.981066262494));
#21263=CARTESIAN_POINT('',(268.41135366976,154.898060492931,258.981066262494));
#21264=CARTESIAN_POINT('Origin',(271.200451731736,150.663111831477,260.573593133705));
#21265=CARTESIAN_POINT('Origin',(271.986847992623,154.073622192239,260.573593133705));
#21266=CARTESIAN_POINT('',(268.518830989589,151.281440556996,259.379197980297));
#21267=CARTESIAN_POINT('Origin',(271.200451731736,150.663111831477,260.573593133705));
#21268=CARTESIAN_POINT('',(268.181804020638,149.819793259527,259.379197980297));
#21269=CARTESIAN_POINT('',(269.305227250476,154.691950917758,259.379197980297));
#21270=CARTESIAN_POINT('Origin',(270.863424762785,149.201464534007,260.573593133705));
#21271=CARTESIAN_POINT('Origin',(271.986847992623,154.073622192239,260.573593133705));
#21272=CARTESIAN_POINT('',(267.287930439922,150.0259028347,258.981066262494));
#21273=CARTESIAN_POINT('Origin',(270.863424762785,149.201464534007,260.573593133705));
#21274=CARTESIAN_POINT('',(258.974598539121,113.971936163789,258.981066262494));
#21275=CARTESIAN_POINT('',(268.41135366976,154.898060492931,258.981066262494));
#21276=CARTESIAN_POINT('Origin',(262.550092861984,113.147497863097,260.573593133705));
#21277=CARTESIAN_POINT('Origin',(271.986847992623,154.073622192239,260.573593133705));
#21278=CARTESIAN_POINT('',(259.868472119837,113.765826588616,259.379197980297));
#21279=CARTESIAN_POINT('Origin',(262.550092861984,113.147497863097,260.573593133705));
#21280=CARTESIAN_POINT('',(259.419102827902,111.816963525324,259.379197980297));
#21281=CARTESIAN_POINT('',(269.305227250476,154.691950917758,259.379197980297));
#21282=CARTESIAN_POINT('Origin',(262.100723570049,111.198634799804,260.573593133705));
#21283=CARTESIAN_POINT('Origin',(271.986847992623,154.073622192239,260.573593133705));
#21284=CARTESIAN_POINT('',(258.525229247186,112.023073100497,258.981066262494));
#21285=CARTESIAN_POINT('Origin',(262.100723570049,111.198634799804,260.573593133705));
#21286=CARTESIAN_POINT('',(258.300544601218,111.048641568851,258.981066262494));
#21287=CARTESIAN_POINT('',(268.41135366976,154.898060492931,258.981066262494));
#21288=CARTESIAN_POINT('Origin',(261.876038924081,110.224203268158,260.573593133705));
#21289=CARTESIAN_POINT('Origin',(261.876038924081,110.224203268158,260.573593133705));
#21290=CARTESIAN_POINT('Origin',(265.676217892912,110.374196499112,262.166120004915));
#21291=CARTESIAN_POINT('Origin',(265.231713604131,112.529169137578,261.767988287112));
#21292=CARTESIAN_POINT('Origin',(274.438919085648,148.377026233315,262.166120004915));
#21293=CARTESIAN_POINT('Origin',(273.882072473883,150.044783105957,261.767988287112));
#21294=CARTESIAN_POINT('Origin',(275.562342315485,153.249183891546,262.166120004915));
#21295=CARTESIAN_POINT('',(0.,0.,0.));
#21296=CARTESIAN_POINT('Origin',(262.314173983718,112.124344754868,260.573593133705));
#21297=CARTESIAN_POINT('',(265.018141565383,111.50086328997,261.777941580057));
#21298=CARTESIAN_POINT('Origin',(265.844974627545,111.310211932935,262.146213419025));
#21299=CARTESIAN_POINT('Origin',(262.314173983718,112.124344754868,260.573593133705));
#21300=CARTESIAN_POINT('',(0.,0.,0.));
#21301=CARTESIAN_POINT('Origin',(263.555188275439,150.886599378764,267.573593133704));
#21302=CARTESIAN_POINT('',(273.299503591901,148.639752919088,255.573593133704));
#21303=CARTESIAN_POINT('',(273.299503591901,148.639752919088,258.306298490302));
#21304=CARTESIAN_POINT('',(273.299503591901,148.639752919088,253.573593133704));
#21305=CARTESIAN_POINT('',(275.248366655194,148.190383627153,253.573593133704));
#21306=CARTESIAN_POINT('',(273.299503591901,148.639752919088,255.573593133704));
#21307=CARTESIAN_POINT('',(278.171661250133,147.51632968925,253.573593133704));
#21308=CARTESIAN_POINT('',(263.555188275439,150.886599378764,253.573593133704));
#21309=CARTESIAN_POINT('',(278.171661250133,147.51632968925,267.573593133704));
#21310=CARTESIAN_POINT('',(278.171661250133,147.51632968925,267.573593133704));
#21311=CARTESIAN_POINT('',(275.248366655194,148.190383627153,267.573593133704));
#21312=CARTESIAN_POINT('',(263.555188275439,150.886599378764,267.573593133704));
#21313=CARTESIAN_POINT('',(273.299503591901,148.639752919088,265.573593133704));
#21314=CARTESIAN_POINT('',(275.248366655194,148.190383627153,267.573593133704));
#21315=CARTESIAN_POINT('',(273.299503591901,148.639752919088,262.840887777106));
#21316=CARTESIAN_POINT('',(273.299503591901,148.639752919088,262.840887777106));
#21317=CARTESIAN_POINT('Origin',(270.863424762786,149.201464534007,260.573593133704));
#21318=CARTESIAN_POINT('Origin',(263.89221524439,152.348246676233,267.573593133704));
#21319=CARTESIAN_POINT('',(275.585393624145,149.652030924622,253.573593133704));
#21320=CARTESIAN_POINT('',(278.508688219084,148.97797698672,253.573593133704));
#21321=CARTESIAN_POINT('',(263.89221524439,152.348246676233,253.573593133704));
#21322=CARTESIAN_POINT('',(273.636530560853,150.101400216558,255.573593133704));
#21323=CARTESIAN_POINT('',(262.917783712744,152.572931322201,266.573593133704));
#21324=CARTESIAN_POINT('',(273.636530560853,150.101400216558,258.306298490302));
#21325=CARTESIAN_POINT('',(273.636530560853,150.101400216558,267.573593133704));
#21326=CARTESIAN_POINT('',(273.636530560853,150.101400216558,262.840887777106));
#21327=CARTESIAN_POINT('Origin',(271.200451731737,150.663111831476,260.573593133704));
#21328=CARTESIAN_POINT('',(273.636530560853,150.101400216558,265.573593133704));
#21329=CARTESIAN_POINT('',(273.636530560853,150.101400216558,267.573593133704));
#21330=CARTESIAN_POINT('',(275.585393624145,149.652030924622,267.573593133704));
#21331=CARTESIAN_POINT('',(269.738804434268,151.000138800428,261.573593133704));
#21332=CARTESIAN_POINT('',(278.508688219084,148.97797698672,267.573593133704));
#21333=CARTESIAN_POINT('',(263.89221524439,152.348246676233,267.573593133704));
#21334=CARTESIAN_POINT('',(278.508688219084,148.97797698672,267.573593133704));
#21335=CARTESIAN_POINT('Origin',(278.958057511019,150.926840050012,267.573593133704));
#21336=CARTESIAN_POINT('',(275.248366655194,148.190383627153,267.573593133704));
#21337=CARTESIAN_POINT('',(282.368567871781,150.140443789126,267.573593133704));
#21338=CARTESIAN_POINT('Origin',(278.958057511019,150.926840050012,267.573593133704));
#21339=CARTESIAN_POINT('',(284.840098977424,160.859190637234,267.573593133704));
#21340=CARTESIAN_POINT('',(282.368567871781,150.140443789126,267.573593133704));
#21341=CARTESIAN_POINT('',(280.716491106192,167.45432961411,267.573593133704));
#21342=CARTESIAN_POINT('Origin',(279.48072555337,162.094956190056,267.573593133704));
#21343=CARTESIAN_POINT('',(269.997744258083,169.925860719754,267.573593133704));
#21344=CARTESIAN_POINT('',(269.997744258083,169.925860719754,267.573593133704));
#21345=CARTESIAN_POINT('',(263.402605281207,165.802252848521,267.573593133704));
#21346=CARTESIAN_POINT('Origin',(268.761978705262,164.566487295699,267.573593133704));
#21347=CARTESIAN_POINT('',(260.931074175564,155.083506000412,267.573593133704));
#21348=CARTESIAN_POINT('',(260.931074175564,155.083506000412,267.573593133704));
#21349=CARTESIAN_POINT('',(263.555188275439,150.886599378764,267.573593133704));
#21350=CARTESIAN_POINT('Origin',(264.341584536326,154.297109739526,267.573593133704));
#21351=CARTESIAN_POINT('',(266.478482870378,150.212545440861,267.573593133704));
#21352=CARTESIAN_POINT('',(263.555188275439,150.886599378764,267.573593133704));
#21353=CARTESIAN_POINT('',(266.815509839329,151.674192738331,267.573593133704));
#21354=CARTESIAN_POINT('',(266.815509839329,151.674192738331,267.573593133704));
#21355=CARTESIAN_POINT('',(263.89221524439,152.348246676233,267.573593133704));
#21356=CARTESIAN_POINT('',(263.89221524439,152.348246676233,267.573593133704));
#21357=CARTESIAN_POINT('',(262.392721473033,154.746479031461,267.573593133704));
#21358=CARTESIAN_POINT('Origin',(264.341584536326,154.297109739526,267.573593133704));
#21359=CARTESIAN_POINT('',(264.864252578677,165.46522587957,267.573593133704));
#21360=CARTESIAN_POINT('',(262.392721473033,154.746479031461,267.573593133704));
#21361=CARTESIAN_POINT('',(269.660717289132,168.464213422284,267.573593133704));
#21362=CARTESIAN_POINT('Origin',(268.761978705262,164.566487295699,267.573593133704));
#21363=CARTESIAN_POINT('',(280.37946413724,165.992682316641,267.573593133704));
#21364=CARTESIAN_POINT('',(269.660717289132,168.464213422284,267.573593133704));
#21365=CARTESIAN_POINT('',(283.378451679955,161.196217606185,267.573593133704));
#21366=CARTESIAN_POINT('Origin',(279.48072555337,162.094956190056,267.573593133704));
#21367=CARTESIAN_POINT('',(280.906920574312,150.477470758077,267.573593133704));
#21368=CARTESIAN_POINT('',(280.906920574312,150.477470758077,267.573593133704));
#21369=CARTESIAN_POINT('Origin',(278.958057511019,150.926840050012,267.573593133704));
#21370=CARTESIAN_POINT('Origin',(278.958057511019,150.926840050012,253.573593133704));
#21371=CARTESIAN_POINT('',(263.89221524439,152.348246676233,253.573593133704));
#21372=CARTESIAN_POINT('',(266.815509839329,151.674192738331,253.573593133704));
#21373=CARTESIAN_POINT('',(263.89221524439,152.348246676233,253.573593133704));
#21374=CARTESIAN_POINT('',(266.478482870378,150.212545440861,253.573593133704));
#21375=CARTESIAN_POINT('',(267.264879131264,153.623055801623,253.573593133704));
#21376=CARTESIAN_POINT('',(263.555188275439,150.886599378764,253.573593133704));
#21377=CARTESIAN_POINT('',(263.555188275439,150.886599378764,253.573593133704));
#21378=CARTESIAN_POINT('',(260.931074175564,155.083506000412,253.573593133704));
#21379=CARTESIAN_POINT('Origin',(264.341584536326,154.297109739526,253.573593133704));
#21380=CARTESIAN_POINT('',(263.402605281207,165.802252848521,253.573593133704));
#21381=CARTESIAN_POINT('',(260.931074175564,155.083506000412,253.573593133704));
#21382=CARTESIAN_POINT('',(269.997744258083,169.925860719754,253.573593133704));
#21383=CARTESIAN_POINT('Origin',(268.761978705262,164.566487295699,253.573593133704));
#21384=CARTESIAN_POINT('',(280.716491106192,167.45432961411,253.573593133704));
#21385=CARTESIAN_POINT('',(269.997744258083,169.925860719754,253.573593133704));
#21386=CARTESIAN_POINT('',(284.840098977424,160.859190637234,253.573593133704));
#21387=CARTESIAN_POINT('Origin',(279.48072555337,162.094956190056,253.573593133704));
#21388=CARTESIAN_POINT('',(282.368567871781,150.140443789126,253.573593133704));
#21389=CARTESIAN_POINT('',(282.368567871781,150.140443789126,253.573593133704));
#21390=CARTESIAN_POINT('Origin',(278.958057511019,150.926840050012,253.573593133704));
#21391=CARTESIAN_POINT('',(276.03476291608,151.600893987915,253.573593133704));
#21392=CARTESIAN_POINT('',(280.906920574312,150.477470758077,253.573593133704));
#21393=CARTESIAN_POINT('Origin',(278.958057511019,150.926840050012,253.573593133704));
#21394=CARTESIAN_POINT('',(283.378451679955,161.196217606185,253.573593133704));
#21395=CARTESIAN_POINT('',(280.906920574312,150.477470758077,253.573593133704));
#21396=CARTESIAN_POINT('',(280.37946413724,165.992682316641,253.573593133704));
#21397=CARTESIAN_POINT('Origin',(279.48072555337,162.094956190056,253.573593133704));
#21398=CARTESIAN_POINT('',(269.660717289132,168.464213422284,253.573593133704));
#21399=CARTESIAN_POINT('',(269.660717289132,168.464213422284,253.573593133704));
#21400=CARTESIAN_POINT('',(264.864252578677,165.46522587957,253.573593133704));
#21401=CARTESIAN_POINT('Origin',(268.761978705262,164.566487295699,253.573593133704));
#21402=CARTESIAN_POINT('',(262.392721473033,154.746479031461,253.573593133704));
#21403=CARTESIAN_POINT('',(262.392721473033,154.746479031461,253.573593133704));
#21404=CARTESIAN_POINT('Origin',(264.341584536326,154.297109739526,253.573593133704));
#21405=CARTESIAN_POINT('Origin',(278.958057511019,150.926840050012,267.573593133704));
#21406=CARTESIAN_POINT('',(282.368567871781,150.140443789126,267.573593133704));
#21407=CARTESIAN_POINT('Origin',(282.368567871781,150.140443789126,267.573593133704));
#21408=CARTESIAN_POINT('',(284.840098977424,160.859190637234,267.573593133704));
#21409=CARTESIAN_POINT('Origin',(279.48072555337,162.094956190056,267.573593133704));
#21410=CARTESIAN_POINT('',(280.716491106192,167.45432961411,267.573593133704));
#21411=CARTESIAN_POINT('Origin',(269.997744258083,169.925860719754,267.573593133704));
#21412=CARTESIAN_POINT('',(269.997744258083,169.925860719754,267.573593133704));
#21413=CARTESIAN_POINT('Origin',(268.761978705262,164.566487295699,267.573593133704));
#21414=CARTESIAN_POINT('',(263.402605281207,165.802252848521,267.573593133704));
#21415=CARTESIAN_POINT('Origin',(260.931074175564,155.083506000412,267.573593133704));
#21416=CARTESIAN_POINT('',(260.931074175564,155.083506000412,267.573593133704));
#21417=CARTESIAN_POINT('Origin',(264.341584536326,154.297109739526,267.573593133704));
#21418=CARTESIAN_POINT('',(263.555188275439,150.886599378764,267.573593133704));
#21419=CARTESIAN_POINT('Origin',(263.555188275439,150.886599378764,267.573593133704));
#21420=CARTESIAN_POINT('',(268.42734593367,149.763176148926,255.573593133704));
#21421=CARTESIAN_POINT('',(266.478482870378,150.212545440861,253.573593133704));
#21422=CARTESIAN_POINT('',(268.42734593367,149.763176148926,258.306298490302));
#21423=CARTESIAN_POINT('',(268.42734593367,149.763176148926,253.573593133704));
#21424=CARTESIAN_POINT('',(268.42734593367,149.763176148926,262.840887777106));
#21425=CARTESIAN_POINT('Origin',(270.863424762786,149.201464534007,260.573593133704));
#21426=CARTESIAN_POINT('',(268.42734593367,149.763176148926,265.573593133704));
#21427=CARTESIAN_POINT('',(268.42734593367,149.763176148926,262.840887777106));
#21428=CARTESIAN_POINT('',(268.42734593367,149.763176148926,265.573593133704));
#21429=CARTESIAN_POINT('Origin',(278.958057511019,150.926840050012,267.573593133704));
#21430=CARTESIAN_POINT('',(280.906920574312,150.477470758077,267.573593133704));
#21431=CARTESIAN_POINT('Origin',(280.906920574312,150.477470758077,267.573593133704));
#21432=CARTESIAN_POINT('',(283.378451679955,161.196217606185,267.573593133704));
#21433=CARTESIAN_POINT('Origin',(279.48072555337,162.094956190056,267.573593133704));
#21434=CARTESIAN_POINT('',(280.37946413724,165.992682316641,267.573593133704));
#21435=CARTESIAN_POINT('Origin',(269.660717289132,168.464213422284,267.573593133704));
#21436=CARTESIAN_POINT('',(269.660717289132,168.464213422284,267.573593133704));
#21437=CARTESIAN_POINT('Origin',(268.761978705262,164.566487295699,267.573593133704));
#21438=CARTESIAN_POINT('',(264.864252578677,165.46522587957,267.573593133704));
#21439=CARTESIAN_POINT('Origin',(262.392721473033,154.746479031461,267.573593133704));
#21440=CARTESIAN_POINT('',(262.392721473033,154.746479031461,267.573593133704));
#21441=CARTESIAN_POINT('Origin',(264.341584536326,154.297109739526,267.573593133704));
#21442=CARTESIAN_POINT('',(263.89221524439,152.348246676233,267.573593133704));
#21443=CARTESIAN_POINT('Origin',(263.89221524439,152.348246676233,267.573593133704));
#21444=CARTESIAN_POINT('',(268.764372902622,151.224823446395,255.573593133704));
#21445=CARTESIAN_POINT('',(268.764372902622,151.224823446395,258.306298490302));
#21446=CARTESIAN_POINT('',(268.764372902622,151.224823446395,267.573593133704));
#21447=CARTESIAN_POINT('',(272.174883263383,150.438427185509,259.073593133704));
#21448=CARTESIAN_POINT('',(268.764372902622,151.224823446395,265.573593133704));
#21449=CARTESIAN_POINT('',(265.35386254186,152.011219707282,269.073593133704));
#21450=CARTESIAN_POINT('',(268.764372902622,151.224823446395,262.840887777106));
#21451=CARTESIAN_POINT('',(268.764372902622,151.224823446395,267.573593133704));
#21452=CARTESIAN_POINT('Origin',(271.200451731737,150.663111831476,260.573593133704));
#21453=CARTESIAN_POINT('Origin',(270.674192393346,159.507491465388,262.840887777106));
#21454=CARTESIAN_POINT('',(268.42734593367,149.763176148926,265.573593133704));
#21455=CARTESIAN_POINT('',(270.674192393346,159.507491465388,262.840887777106));
#21456=CARTESIAN_POINT('Origin',(273.110271222462,158.945779850469,260.573593133704));
#21457=CARTESIAN_POINT('',(270.674192393346,159.507491465388,258.306298490302));
#21458=CARTESIAN_POINT('Origin',(270.674192393346,159.507491465388,253.573593133704));
#21459=CARTESIAN_POINT('',(270.674192393346,159.507491465388,255.573593133704));
#21460=CARTESIAN_POINT('Origin',(275.546350051577,158.38406823555,262.840887777106));
#21461=CARTESIAN_POINT('',(273.636530560853,150.101400216558,265.573593133704));
#21462=CARTESIAN_POINT('',(275.546350051577,158.38406823555,262.840887777106));
#21463=CARTESIAN_POINT('Origin',(273.110271222462,158.945779850469,260.573593133704));
#21464=CARTESIAN_POINT('',(275.546350051577,158.38406823555,258.306298490302));
#21465=CARTESIAN_POINT('Origin',(275.546350051577,158.38406823555,253.573593133704));
#21466=CARTESIAN_POINT('',(275.546350051577,158.38406823555,255.573593133704));
#21467=CARTESIAN_POINT('Origin',(267.264879131264,153.623055801623,253.573593133704));
#21468=CARTESIAN_POINT('Origin',(275.546350051577,158.38406823555,255.573593133704));
#21469=CARTESIAN_POINT('Origin',(276.03476291608,151.600893987915,267.573593133704));
#21470=CARTESIAN_POINT('Origin',(270.674192393346,159.507491465388,265.573593133704));
#21471=CARTESIAN_POINT('',(0.,0.,0.));
#21472=CARTESIAN_POINT('Ctrl Pts',(241.704224565777,155.65704992868,244.573619803768));
#21473=CARTESIAN_POINT('Ctrl Pts',(241.510068395548,155.841112484094,244.574122853875));
#21474=CARTESIAN_POINT('Ctrl Pts',(241.271802936649,155.964045706855,244.684411798912));
#21475=CARTESIAN_POINT('Ctrl Pts',(240.885055878546,156.088013810182,245.049510693237));
#21476=CARTESIAN_POINT('Ctrl Pts',(240.747008314468,156.102746965415,245.307955179719));
#21477=CARTESIAN_POINT('Ctrl Pts',(240.747915979192,156.102607114311,245.84060223374));
#21478=CARTESIAN_POINT('Ctrl Pts',(240.88541559932,156.087955834116,246.097804076277));
#21479=CARTESIAN_POINT('Ctrl Pts',(241.272276604401,155.963830882667,246.463437960953));
#21480=CARTESIAN_POINT('Ctrl Pts',(241.511138824461,155.840473431548,246.573503411772));
#21481=CARTESIAN_POINT('Ctrl Pts',(241.899470444745,155.471564785668,246.573627286256));
#21482=CARTESIAN_POINT('Ctrl Pts',(242.031853219533,155.239145808301,246.462784974605));
#21483=CARTESIAN_POINT('Ctrl Pts',(242.173429602105,154.859535412975,246.097307277076));
#21484=CARTESIAN_POINT('Ctrl Pts',(242.194992380974,154.72208775409,245.8387163343));
#21485=CARTESIAN_POINT('Ctrl Pts',(242.19477499151,154.723076345322,245.306032501962));
#21486=CARTESIAN_POINT('Ctrl Pts',(242.173220430076,154.860146597241,245.049124108673));
#21487=CARTESIAN_POINT('Ctrl Pts',(242.031625185487,155.239682567333,244.684046451652));
#21488=CARTESIAN_POINT('Ctrl Pts',(241.898380736007,155.472987373266,244.573116753661));
#21489=CARTESIAN_POINT('Ctrl Pts',(241.704224565777,155.65704992868,244.573619803768));
#21490=CARTESIAN_POINT('Ctrl Pts',(242.051749888954,156.021528794222,244.070014088572));
#21491=CARTESIAN_POINT('Ctrl Pts',(241.718234113437,156.338315834566,244.070770482515));
#21492=CARTESIAN_POINT('Ctrl Pts',(241.338489677445,156.581146969436,244.236602955261));
#21493=CARTESIAN_POINT('Ctrl Pts',(240.743859410108,156.868106208125,244.785572840259));
#21494=CARTESIAN_POINT('Ctrl Pts',(240.540094008181,156.928680846509,245.174179737123));
#21495=CARTESIAN_POINT('Ctrl Pts',(240.541446108007,156.928221627357,245.975068211741));
#21496=CARTESIAN_POINT('Ctrl Pts',(240.744396066514,156.867920564623,246.361806700368));
#21497=CARTESIAN_POINT('Ctrl Pts',(241.339235998406,156.58070622062,246.911580897118));
#21498=CARTESIAN_POINT('Ctrl Pts',(241.719963975899,156.33710291391,247.077077359117));
#21499=CARTESIAN_POINT('Ctrl Pts',(242.387250650439,155.702410355244,247.077263646609));
#21500=CARTESIAN_POINT('Ctrl Pts',(242.645427060325,155.334768929497,246.910599101822));
#21501=CARTESIAN_POINT('Ctrl Pts',(242.959181374525,154.755791378006,246.361059656098));
#21502=CARTESIAN_POINT('Ctrl Pts',(243.029858527513,154.554695114521,245.972232660372));
#21503=CARTESIAN_POINT('Ctrl Pts',(243.029260143558,154.556159389752,245.171288638899));
#21504=CARTESIAN_POINT('Ctrl Pts',(242.958703359359,154.756718137498,244.784991571802));
#21505=CARTESIAN_POINT('Ctrl Pts',(242.644943159656,155.335595609506,244.23605360463));
#21506=CARTESIAN_POINT('Ctrl Pts',(242.385265664471,155.704741753878,244.06925769463));
#21507=CARTESIAN_POINT('Ctrl Pts',(242.051749888954,156.021528794222,244.070014088572));
#21508=CARTESIAN_POINT('',(241.704241838302,155.657068046185,246.573593133381));
#21509=CARTESIAN_POINT('',(241.704242970102,155.657069230833,244.573593133703));
#21510=CARTESIAN_POINT('Ctrl Pts',(241.704241838524,155.657068046418,246.573593133703));
#21511=CARTESIAN_POINT('Ctrl Pts',(241.736872664963,155.626024791641,246.573593133777));
#21512=CARTESIAN_POINT('Ctrl Pts',(241.767882349574,155.59363497048,246.570551147));
#21513=CARTESIAN_POINT('Ctrl Pts',(241.826534715335,155.526925812411,246.558577698866));
#21514=CARTESIAN_POINT('Ctrl Pts',(241.854090414984,155.492712431425,246.549670593028));
#21515=CARTESIAN_POINT('Ctrl Pts',(241.931937847661,155.387937570196,246.514389597396));
#21516=CARTESIAN_POINT('Ctrl Pts',(241.976284330344,155.316540049691,246.47971112174));
#21517=CARTESIAN_POINT('Ctrl Pts',(242.038432360623,155.199911928688,246.405940491082));
#21518=CARTESIAN_POINT('Ctrl Pts',(242.060099761803,155.153899400574,246.372086195779));
#21519=CARTESIAN_POINT('Ctrl Pts',(242.089421604343,155.084219718394,246.313003139576));
#21520=CARTESIAN_POINT('Ctrl Pts',(242.099060009831,155.059307245471,246.290206730024));
#21521=CARTESIAN_POINT('Ctrl Pts',(242.116743454559,155.011184520392,246.242334167609));
#21522=CARTESIAN_POINT('Ctrl Pts',(242.124923515658,154.987810179667,246.216956137048));
#21523=CARTESIAN_POINT('Ctrl Pts',(242.146344100199,154.92364651811,246.140681005568));
#21524=CARTESIAN_POINT('Ctrl Pts',(242.157701589958,154.885595585108,246.086958711194));
#21525=CARTESIAN_POINT('Ctrl Pts',(242.174748890245,154.822521444716,245.978032102338));
#21526=CARTESIAN_POINT('Ctrl Pts',(242.180851754483,154.796652641199,245.923416774259));
#21527=CARTESIAN_POINT('Ctrl Pts',(242.192502243845,154.741829624733,245.772513348259));
#21528=CARTESIAN_POINT('Ctrl Pts',(242.19491685745,154.722482122952,245.673483077984));
#21529=CARTESIAN_POINT('Ctrl Pts',(242.194939339411,154.722662003917,245.473008288348));
#21530=CARTESIAN_POINT('Ctrl Pts',(242.192458196941,154.74191321076,245.374193081089));
#21531=CARTESIAN_POINT('Ctrl Pts',(242.18073855789,154.796791362237,245.223303692942));
#21532=CARTESIAN_POINT('Ctrl Pts',(242.174629050872,154.822651099648,245.16876516982));
#21533=CARTESIAN_POINT('Ctrl Pts',(242.15759229929,154.885742196139,245.059926304006));
#21534=CARTESIAN_POINT('Ctrl Pts',(242.146250544142,154.92382744045,245.006226072546));
#21535=CARTESIAN_POINT('Ctrl Pts',(242.124835141528,154.988050584937,244.929954836604));
#21536=CARTESIAN_POINT('Ctrl Pts',(242.116647203304,155.011461461694,244.904560232997));
#21537=CARTESIAN_POINT('Ctrl Pts',(242.098943859986,155.059603438356,244.856699719665));
#21538=CARTESIAN_POINT('Ctrl Pts',(242.089314088538,155.084472314344,244.833955999992));
#21539=CARTESIAN_POINT('Ctrl Pts',(242.060018432519,155.154093511846,244.774957037284));
#21540=CARTESIAN_POINT('Ctrl Pts',(242.038370261862,155.200086959791,244.741137633888));
#21541=CARTESIAN_POINT('Ctrl Pts',(241.976228876202,155.316724936344,244.667392469806));
#21542=CARTESIAN_POINT('Ctrl Pts',(241.931856584362,155.388139210515,244.632719291294));
#21543=CARTESIAN_POINT('Ctrl Pts',(241.853959577504,155.492909761618,244.597463836825));
#21544=CARTESIAN_POINT('Ctrl Pts',(241.826400985401,155.527101906926,244.588569745954));
#21545=CARTESIAN_POINT('Ctrl Pts',(241.767780801273,155.593738280963,244.576624852807));
#21546=CARTESIAN_POINT('Ctrl Pts',(241.736817627638,155.626071525356,244.573593133703));
#21547=CARTESIAN_POINT('Ctrl Pts',(241.704242970102,155.657069230833,244.573593133703));
#21548=CARTESIAN_POINT('',(242.049277846445,156.018936140718,247.073589514835));
#21549=CARTESIAN_POINT('',(241.704240380882,155.657066517399,246.573591021215));
#21550=CARTESIAN_POINT('',(242.049280067237,156.018938485669,244.073593137428));
#21551=CARTESIAN_POINT('Ctrl Pts',(242.04928006672,156.018938485126,244.073593133703));
#21552=CARTESIAN_POINT('Ctrl Pts',(242.219085177029,155.857031770043,244.073325863255));
#21553=CARTESIAN_POINT('Ctrl Pts',(242.363945625518,155.690456210395,244.109847139091));
#21554=CARTESIAN_POINT('Ctrl Pts',(242.548946094757,155.444153214881,244.219811905837));
#21555=CARTESIAN_POINT('Ctrl Pts',(242.605251765288,155.362612438805,244.265663970251));
#21556=CARTESIAN_POINT('Ctrl Pts',(242.708167559415,155.202029405512,244.37576238341));
#21557=CARTESIAN_POINT('Ctrl Pts',(242.753983429964,155.124439488524,244.438626167558));
#21558=CARTESIAN_POINT('Ctrl Pts',(242.883294398959,154.888388370452,244.663127176969));
#21559=CARTESIAN_POINT('Ctrl Pts',(242.937958626695,154.765039089602,244.826245103114));
#21560=CARTESIAN_POINT('Ctrl Pts',(243.008010283782,154.599423235233,245.17938212848));
#21561=CARTESIAN_POINT('Ctrl Pts',(243.023489700801,154.556974142855,245.369501892319));
#21562=CARTESIAN_POINT('Ctrl Pts',(243.023766909856,154.556251500951,245.776239362339));
#21563=CARTESIAN_POINT('Ctrl Pts',(243.008413092906,154.598417281956,245.966395214971));
#21564=CARTESIAN_POINT('Ctrl Pts',(242.955809418766,154.722862723227,246.231809670352));
#21565=CARTESIAN_POINT('Ctrl Pts',(242.93321176695,154.774491255809,246.316977934885));
#21566=CARTESIAN_POINT('Ctrl Pts',(242.889789275449,154.866206518623,246.439775500791));
#21567=CARTESIAN_POINT('Ctrl Pts',(242.873719911226,154.899151839497,246.479882217612));
#21568=CARTESIAN_POINT('Ctrl Pts',(242.837984377284,154.969559473606,246.558444040955));
#21569=CARTESIAN_POINT('Ctrl Pts',(242.817773280998,155.008015020619,246.597842459808));
#21570=CARTESIAN_POINT('Ctrl Pts',(242.627600826482,155.354975670536,246.927734975046));
#21571=CARTESIAN_POINT('Ctrl Pts',(242.389986925115,155.694079425826,247.074098313406));
#21572=CARTESIAN_POINT('Ctrl Pts',(242.049278403401,156.018936725024,247.073589666413));
#21573=CARTESIAN_POINT('',(241.704242970102,155.657069230833,244.573593133703));
#21574=CARTESIAN_POINT('Ctrl Pts',(236.873741527621,150.590918454637,244.573619803768));
#21575=CARTESIAN_POINT('Ctrl Pts',(237.06789769785,150.406855899223,244.574122853875));
#21576=CARTESIAN_POINT('Ctrl Pts',(237.306163156749,150.283922676462,244.684411798912));
#21577=CARTESIAN_POINT('Ctrl Pts',(237.692910214852,150.159954573134,245.049510693237));
#21578=CARTESIAN_POINT('Ctrl Pts',(237.83095777893,150.145221417902,245.307955179719));
#21579=CARTESIAN_POINT('Ctrl Pts',(237.830050114206,150.145361269005,245.84060223374));
#21580=CARTESIAN_POINT('Ctrl Pts',(237.692550494078,150.1600125492,246.097804076277));
#21581=CARTESIAN_POINT('Ctrl Pts',(237.305689488997,150.28413750065,246.463437960953));
#21582=CARTESIAN_POINT('Ctrl Pts',(237.066827268937,150.407494951768,246.573503411772));
#21583=CARTESIAN_POINT('Ctrl Pts',(236.678495648654,150.776403597648,246.573627286256));
#21584=CARTESIAN_POINT('Ctrl Pts',(236.546112873865,151.008822575015,246.462784974605));
#21585=CARTESIAN_POINT('Ctrl Pts',(236.404536491293,151.388432970342,246.097307277076));
#21586=CARTESIAN_POINT('Ctrl Pts',(236.382973712424,151.525880629227,245.8387163343));
#21587=CARTESIAN_POINT('Ctrl Pts',(236.383191101889,151.524892037994,245.306032501962));
#21588=CARTESIAN_POINT('Ctrl Pts',(236.404745663322,151.387821786076,245.049124108673));
#21589=CARTESIAN_POINT('Ctrl Pts',(236.546340907911,151.008285815983,244.684046451652));
#21590=CARTESIAN_POINT('Ctrl Pts',(236.679585357392,150.774981010051,244.573116753661));
#21591=CARTESIAN_POINT('Ctrl Pts',(236.873741527621,150.590918454637,244.573619803768));
#21592=CARTESIAN_POINT('Ctrl Pts',(236.526170038182,150.226391170675,244.069947188143));
#21593=CARTESIAN_POINT('Ctrl Pts',(236.859704326629,149.909586498829,244.07070361574));
#21594=CARTESIAN_POINT('Ctrl Pts',(237.239467557095,149.666739436376,244.236543467048));
#21595=CARTESIAN_POINT('Ctrl Pts',(237.834125440234,149.379758545477,244.785537777997));
#21596=CARTESIAN_POINT('Ctrl Pts',(238.037899572308,149.319177817379,245.174161966009));
#21597=CARTESIAN_POINT('Ctrl Pts',(238.036547413442,149.319637078956,245.975086074588));
#21598=CARTESIAN_POINT('Ctrl Pts',(237.833588760324,149.379944205939,246.361841771235));
#21599=CARTESIAN_POINT('Ctrl Pts',(237.238721199914,149.667180215205,246.911640429713));
#21600=CARTESIAN_POINT('Ctrl Pts',(236.857974376567,149.91079949572,247.077144255326));
#21601=CARTESIAN_POINT('Ctrl Pts',(236.190650644836,150.545527361884,247.07733055111));
#21602=CARTESIAN_POINT('Ctrl Pts',(235.932457524162,150.913186750969,246.910658590737));
#21603=CARTESIAN_POINT('Ctrl Pts',(235.61868033735,151.492190786966,246.361094693722));
#21604=CARTESIAN_POINT('Ctrl Pts',(235.547996659869,151.693295505715,245.972250397064));
#21605=CARTESIAN_POINT('Ctrl Pts',(235.548595094435,151.691831167293,245.171270739137));
#21606=CARTESIAN_POINT('Ctrl Pts',(235.619158388231,151.491263985552,244.784956483677));
#21607=CARTESIAN_POINT('Ctrl Pts',(235.932941458821,150.912360032447,244.235994091974));
#21608=CARTESIAN_POINT('Ctrl Pts',(236.192635749735,150.543195842521,244.069190760545));
#21609=CARTESIAN_POINT('Ctrl Pts',(236.526170038182,150.226391170675,244.069947188143));
#21610=CARTESIAN_POINT('',(236.873724255103,150.590900337126,246.573593133381));
#21611=CARTESIAN_POINT('',(236.873723123297,150.590899152483,244.573593133703));
#21612=CARTESIAN_POINT('Ctrl Pts',(236.873724254881,150.590900336893,246.573593133703));
#21613=CARTESIAN_POINT('Ctrl Pts',(236.84109342844,150.621943591671,246.573593133777));
#21614=CARTESIAN_POINT('Ctrl Pts',(236.810083743827,150.654333412834,246.570551147));
#21615=CARTESIAN_POINT('Ctrl Pts',(236.751431378063,150.721042570906,246.558577698866));
#21616=CARTESIAN_POINT('Ctrl Pts',(236.723875678414,150.755255951892,246.549670593028));
#21617=CARTESIAN_POINT('Ctrl Pts',(236.646028245737,150.860030813121,246.514389597396));
#21618=CARTESIAN_POINT('Ctrl Pts',(236.601681763054,150.931428333627,246.47971112174));
#21619=CARTESIAN_POINT('Ctrl Pts',(236.539533732776,151.048056454629,246.405940491082));
#21620=CARTESIAN_POINT('Ctrl Pts',(236.517866331595,151.094068982743,246.372086195779));
#21621=CARTESIAN_POINT('Ctrl Pts',(236.488544489055,151.163748664924,246.313003139575));
#21622=CARTESIAN_POINT('Ctrl Pts',(236.478906083567,151.188661137847,246.290206730023));
#21623=CARTESIAN_POINT('Ctrl Pts',(236.461222638839,151.236783862925,246.242334167609));
#21624=CARTESIAN_POINT('Ctrl Pts',(236.453042577741,151.26015820365,246.216956137048));
#21625=CARTESIAN_POINT('Ctrl Pts',(236.431621993199,151.324321865207,246.140681005568));
#21626=CARTESIAN_POINT('Ctrl Pts',(236.42026450344,151.362372798209,246.086958711194));
#21627=CARTESIAN_POINT('Ctrl Pts',(236.403217203154,151.4254469386,245.978032102337));
#21628=CARTESIAN_POINT('Ctrl Pts',(236.397114338915,151.451315742117,245.923416774258));
#21629=CARTESIAN_POINT('Ctrl Pts',(236.385463849553,151.506138758584,245.772513348258));
#21630=CARTESIAN_POINT('Ctrl Pts',(236.383049235948,151.525486260365,245.673483077983));
#21631=CARTESIAN_POINT('Ctrl Pts',(236.383026753987,151.5253063794,245.473008288348));
#21632=CARTESIAN_POINT('Ctrl Pts',(236.385507896457,151.506055172556,245.374193081089));
#21633=CARTESIAN_POINT('Ctrl Pts',(236.397227535509,151.45117702108,245.223303692942));
#21634=CARTESIAN_POINT('Ctrl Pts',(236.403337042526,151.425317283669,245.16876516982));
#21635=CARTESIAN_POINT('Ctrl Pts',(236.420373794109,151.362226187178,245.059926304005));
#21636=CARTESIAN_POINT('Ctrl Pts',(236.431715549256,151.324140942867,245.006226072545));
#21637=CARTESIAN_POINT('Ctrl Pts',(236.45313095187,151.25991779838,244.929954836604));
#21638=CARTESIAN_POINT('Ctrl Pts',(236.461318890094,151.236506921622,244.904560232997));
#21639=CARTESIAN_POINT('Ctrl Pts',(236.479022233412,151.188364944961,244.856699719665));
#21640=CARTESIAN_POINT('Ctrl Pts',(236.488652004861,151.163496068973,244.833955999992));
#21641=CARTESIAN_POINT('Ctrl Pts',(236.517947660879,151.09387487147,244.774957037284));
#21642=CARTESIAN_POINT('Ctrl Pts',(236.539595831537,151.047881423526,244.741137633888));
#21643=CARTESIAN_POINT('Ctrl Pts',(236.601737217197,150.931243446973,244.667392469806));
#21644=CARTESIAN_POINT('Ctrl Pts',(236.646109509036,150.859829172802,244.632719291294));
#21645=CARTESIAN_POINT('Ctrl Pts',(236.724006515894,150.755058621699,244.597463836825));
#21646=CARTESIAN_POINT('Ctrl Pts',(236.751565107997,150.720866476391,244.588569745954));
#21647=CARTESIAN_POINT('Ctrl Pts',(236.810185292125,150.654230102354,244.576624852807));
#21648=CARTESIAN_POINT('Ctrl Pts',(236.841148465761,150.621896857961,244.573593133703));
#21649=CARTESIAN_POINT('Ctrl Pts',(236.873723123297,150.590899152483,244.573593133703));
#21650=CARTESIAN_POINT('',(236.528689854778,150.229030713486,247.073589202258));
#21651=CARTESIAN_POINT('',(236.873725712516,150.590901865917,246.573591021215));
#21652=CARTESIAN_POINT('',(236.528686026161,150.229029897647,244.073593137428));
#21653=CARTESIAN_POINT('Ctrl Pts',(236.528686026679,150.229029898191,244.073593133703));
#21654=CARTESIAN_POINT('Ctrl Pts',(236.358977792143,150.390844243626,244.073207336743));
#21655=CARTESIAN_POINT('Ctrl Pts',(236.214147012029,150.557360059161,244.109671982816));
#21656=CARTESIAN_POINT('Ctrl Pts',(236.029129074192,150.80366177929,244.219644650044));
#21657=CARTESIAN_POINT('Ctrl Pts',(235.972807292529,150.88521660712,244.26551482214));
#21658=CARTESIAN_POINT('Ctrl Pts',(235.86984508284,151.045860635605,244.375680399037));
#21659=CARTESIAN_POINT('Ctrl Pts',(235.823963573414,151.123561960789,244.438654405421));
#21660=CARTESIAN_POINT('Ctrl Pts',(235.694654847654,151.359614330903,244.663166238249));
#21661=CARTESIAN_POINT('Ctrl Pts',(235.639993226236,151.482961305671,244.826292334005));
#21662=CARTESIAN_POINT('Ctrl Pts',(235.569947693597,151.648565991774,245.179447606592));
#21663=CARTESIAN_POINT('Ctrl Pts',(235.554471743642,151.691006359538,245.369584971744));
#21664=CARTESIAN_POINT('Ctrl Pts',(235.554203716487,151.691705065711,245.776329368437));
#21665=CARTESIAN_POINT('Ctrl Pts',(235.569563174184,151.649524262202,245.966487747264));
#21666=CARTESIAN_POINT('Ctrl Pts',(235.622179572538,151.525052876751,246.231904586228));
#21667=CARTESIAN_POINT('Ctrl Pts',(235.644782194467,151.473415137899,246.317073411003));
#21668=CARTESIAN_POINT('Ctrl Pts',(235.688213704026,151.381685522078,246.439871465846));
#21669=CARTESIAN_POINT('Ctrl Pts',(235.704286335514,151.348735327601,246.479978287074));
#21670=CARTESIAN_POINT('Ctrl Pts',(235.740029011678,151.278317835617,246.55854020209));
#21671=CARTESIAN_POINT('Ctrl Pts',(235.760244184763,151.239857072587,246.597938651966));
#21672=CARTESIAN_POINT('Ctrl Pts',(235.950439876362,150.892877130181,246.927807707392));
#21673=CARTESIAN_POINT('Ctrl Pts',(236.187731957931,150.554124308018,247.074228761836));
#21674=CARTESIAN_POINT('Ctrl Pts',(236.528689297355,150.229030128645,247.073589199254));
#21675=CARTESIAN_POINT('',(236.873723123297,150.590899152483,244.573593133703));
#21676=CARTESIAN_POINT('Origin',(242.04928006672,156.018938485126,245.573593133703));
#21677=CARTESIAN_POINT('Ctrl Pts',(241.704242970102,155.657069230833,244.573593133703));
#21678=CARTESIAN_POINT('Ctrl Pts',(241.630962824868,155.726801855244,244.573593133703));
#21679=CARTESIAN_POINT('Ctrl Pts',(241.551605382331,155.78805678601,244.588926668372));
#21680=CARTESIAN_POINT('Ctrl Pts',(241.443050901967,155.858045218471,244.628234491494));
#21681=CARTESIAN_POINT('Ctrl Pts',(241.415780822802,155.874503493771,244.639604524938));
#21682=CARTESIAN_POINT('Ctrl Pts',(241.272162238111,155.955893693544,244.707242077006));
#21683=CARTESIAN_POINT('Ctrl Pts',(241.164964889003,155.998554010553,244.784746950616));
#21684=CARTESIAN_POINT('Ctrl Pts',(241.063791249207,156.030721162401,244.880838247272));
#21685=CARTESIAN_POINT('Ctrl Pts',(241.051524170799,156.034520712982,244.89301514354));
#21686=CARTESIAN_POINT('Ctrl Pts',(241.02744274686,156.041789826092,244.918011816567));
#21687=CARTESIAN_POINT('Ctrl Pts',(241.015630708891,156.045257826393,244.930834103936));
#21688=CARTESIAN_POINT('Ctrl Pts',(240.960645876954,156.06096670119,244.993308664963));
#21689=CARTESIAN_POINT('Ctrl Pts',(240.921101198906,156.070922047133,245.04672122124));
#21690=CARTESIAN_POINT('Ctrl Pts',(240.855267036901,156.085703737406,245.155343526424));
#21691=CARTESIAN_POINT('Ctrl Pts',(240.82813302031,156.090901164723,245.20995619415));
#21692=CARTESIAN_POINT('Ctrl Pts',(240.786741009928,156.097888240926,245.317836348554));
#21693=CARTESIAN_POINT('Ctrl Pts',(240.771507778469,156.099964606954,245.37057049282));
#21694=CARTESIAN_POINT('Ctrl Pts',(240.752244886547,156.102294553641,245.473637636456));
#21695=CARTESIAN_POINT('Ctrl Pts',(240.747419389518,156.102688907628,245.52350987106));
#21696=CARTESIAN_POINT('Ctrl Pts',(240.747508336191,156.102780888958,245.66744290748));
#21697=CARTESIAN_POINT('Ctrl Pts',(240.764538417831,156.101609329828,245.766443228677));
#21698=CARTESIAN_POINT('Ctrl Pts',(240.822244927711,156.092107051219,245.923804651633));
#21699=CARTESIAN_POINT('Ctrl Pts',(240.848360549117,156.087222664751,245.978365805299));
#21700=CARTESIAN_POINT('Ctrl Pts',(240.912182483255,156.073188120536,246.087229534118));
#21701=CARTESIAN_POINT('Ctrl Pts',(240.95075681251,156.063667434727,246.140929653169));
#21702=CARTESIAN_POINT('Ctrl Pts',(241.01592973934,156.045337831578,246.21720597302));
#21703=CARTESIAN_POINT('Ctrl Pts',(241.039710474856,156.038276122433,246.242605470456));
#21704=CARTESIAN_POINT('Ctrl Pts',(241.08864266278,156.022897012116,246.290460601381));
#21705=CARTESIAN_POINT('Ctrl Pts',(241.11395054769,156.014462688202,246.313212577001));
#21706=CARTESIAN_POINT('Ctrl Pts',(241.184850160234,155.988500534368,246.372197845411));
#21707=CARTESIAN_POINT('Ctrl Pts',(241.231762406002,155.969048729803,246.406000105603));
#21708=CARTESIAN_POINT('Ctrl Pts',(241.315513812164,155.929351171955,246.457744032173));
#21709=CARTESIAN_POINT('Ctrl Pts',(241.351844268562,155.910582668646,246.477508148981));
#21710=CARTESIAN_POINT('Ctrl Pts',(241.415584476112,155.874491292809,246.507530839585));
#21711=CARTESIAN_POINT('Ctrl Pts',(241.442873673692,155.858037293914,246.518909668632));
#21712=CARTESIAN_POINT('Ctrl Pts',(241.551506550977,155.78806465653,246.558247879177));
#21713=CARTESIAN_POINT('Ctrl Pts',(241.630918492936,155.726824027084,246.573593133538));
#21714=CARTESIAN_POINT('Ctrl Pts',(241.704241838524,155.657068046418,246.573593133703));
#21715=CARTESIAN_POINT('',(242.04928006672,156.018938485126,246.573593133703));
#21716=CARTESIAN_POINT('Ctrl Pts',(236.873723123297,150.590899152483,244.573593133703));
#21717=CARTESIAN_POINT('Ctrl Pts',(236.94700326853,150.521166528072,244.573593133703));
#21718=CARTESIAN_POINT('Ctrl Pts',(237.026360711067,150.459911597307,244.588926668372));
#21719=CARTESIAN_POINT('Ctrl Pts',(237.134915191431,150.389923164846,244.628234491494));
#21720=CARTESIAN_POINT('Ctrl Pts',(237.162185270595,150.373464889546,244.639604524937));
#21721=CARTESIAN_POINT('Ctrl Pts',(237.305803855289,150.292074689772,244.707242077007));
#21722=CARTESIAN_POINT('Ctrl Pts',(237.413001204397,150.249414372764,244.784746950618));
#21723=CARTESIAN_POINT('Ctrl Pts',(237.514174844192,150.217247220916,244.880838247272));
#21724=CARTESIAN_POINT('Ctrl Pts',(237.526441922599,150.213447670335,244.89301514354));
#21725=CARTESIAN_POINT('Ctrl Pts',(237.550523346536,150.206178557225,244.918011816565));
#21726=CARTESIAN_POINT('Ctrl Pts',(237.562335384507,150.202710556923,244.930834103935));
#21727=CARTESIAN_POINT('Ctrl Pts',(237.617320216445,150.187001682126,244.993308664963));
#21728=CARTESIAN_POINT('Ctrl Pts',(237.656864894493,150.177046336184,245.046721221241));
#21729=CARTESIAN_POINT('Ctrl Pts',(237.722699056497,150.162264645911,245.155343526424));
#21730=CARTESIAN_POINT('Ctrl Pts',(237.749833073088,150.157067218594,245.20995619415));
#21731=CARTESIAN_POINT('Ctrl Pts',(237.79122508347,150.150080142391,245.317836348554));
#21732=CARTESIAN_POINT('Ctrl Pts',(237.80645831493,150.148003776363,245.37057049282));
#21733=CARTESIAN_POINT('Ctrl Pts',(237.825721206852,150.145673829676,245.473637636457));
#21734=CARTESIAN_POINT('Ctrl Pts',(237.83054670388,150.145279475689,245.52350987106));
#21735=CARTESIAN_POINT('Ctrl Pts',(237.830457757208,150.145187494359,245.667442907476));
#21736=CARTESIAN_POINT('Ctrl Pts',(237.813427675569,150.146359053489,245.766443228673));
#21737=CARTESIAN_POINT('Ctrl Pts',(237.755721165688,150.155861332098,245.923804651633));
#21738=CARTESIAN_POINT('Ctrl Pts',(237.729605544281,150.160745718566,245.978365805299));
#21739=CARTESIAN_POINT('Ctrl Pts',(237.665783610144,150.17478026278,246.087229534118));
#21740=CARTESIAN_POINT('Ctrl Pts',(237.627209280889,150.18430094859,246.140929653169));
#21741=CARTESIAN_POINT('Ctrl Pts',(237.562036354058,150.202630551739,246.21720597302));
#21742=CARTESIAN_POINT('Ctrl Pts',(237.538255618541,150.209692260884,246.242605470456));
#21743=CARTESIAN_POINT('Ctrl Pts',(237.489323430618,150.225071371201,246.290460601382));
#21744=CARTESIAN_POINT('Ctrl Pts',(237.464015545708,150.233505695115,246.313212577001));
#21745=CARTESIAN_POINT('Ctrl Pts',(237.393115933165,150.259467848949,246.372197845411));
#21746=CARTESIAN_POINT('Ctrl Pts',(237.346203687396,150.278919653514,246.406000105603));
#21747=CARTESIAN_POINT('Ctrl Pts',(237.262452281233,150.318617211362,246.457744032174));
#21748=CARTESIAN_POINT('Ctrl Pts',(237.226121824836,150.337385714671,246.477508148981));
#21749=CARTESIAN_POINT('Ctrl Pts',(237.162381617287,150.373477090508,246.507530839585));
#21750=CARTESIAN_POINT('Ctrl Pts',(237.135092419706,150.389931089402,246.518909668632));
#21751=CARTESIAN_POINT('Ctrl Pts',(237.026459542421,150.459903726787,246.558247879178));
#21752=CARTESIAN_POINT('Ctrl Pts',(236.947047600469,150.521144356227,246.573593133537));
#21753=CARTESIAN_POINT('Ctrl Pts',(236.873724254881,150.590900336893,246.573593133703));
#21754=CARTESIAN_POINT('Origin',(239.288983046699,153.123984191658,244.073593133703));
#21755=CARTESIAN_POINT('Origin',(239.288983046699,153.123984191658,244.073593133703));
#21756=CARTESIAN_POINT('',(241.252450952944,155.183237164813,242.073593133703));
#21757=CARTESIAN_POINT('',(242.04928006672,156.018938485126,244.073593133703));
#21758=CARTESIAN_POINT('Origin',(239.288983046699,153.123984191658,242.073593133703));
#21759=CARTESIAN_POINT('Origin',(239.288983046699,153.123984191658,244.073593133703));
#21760=CARTESIAN_POINT('Origin',(239.288983046699,153.123984191658,275.073593133703));
#21761=CARTESIAN_POINT('',(242.04928006672,156.018938485126,271.473593133703));
#21762=CARTESIAN_POINT('Origin',(239.288983046699,153.123984191658,271.473593133703));
#21763=CARTESIAN_POINT('',(242.04928006672,156.018938485126,275.073593133703));
#21764=CARTESIAN_POINT('Ctrl Pts',(242.049278403401,156.018936725024,247.073589666413));
#21765=CARTESIAN_POINT('Ctrl Pts',(241.879080979887,156.181220851564,247.073336255209));
#21766=CARTESIAN_POINT('Ctrl Pts',(241.70548469323,156.318159568681,247.036490765957));
#21767=CARTESIAN_POINT('Ctrl Pts',(241.450419954028,156.491290181965,246.926335097092));
#21768=CARTESIAN_POINT('Ctrl Pts',(241.366251820411,156.543639888291,246.880468634973));
#21769=CARTESIAN_POINT('Ctrl Pts',(241.200961977391,156.638728451252,246.770439899073));
#21770=CARTESIAN_POINT('Ctrl Pts',(241.121296005925,156.68075993574,246.707630692229));
#21771=CARTESIAN_POINT('Ctrl Pts',(240.879699838575,156.798452586541,246.48357204053));
#21772=CARTESIAN_POINT('Ctrl Pts',(240.754085054325,156.847092028425,246.320599865048));
#21773=CARTESIAN_POINT('Ctrl Pts',(240.585611844582,156.909061419067,245.967456032054));
#21774=CARTESIAN_POINT('Ctrl Pts',(240.542567166162,156.922474283323,245.777012017024));
#21775=CARTESIAN_POINT('Ctrl Pts',(240.541906382068,156.922692292675,245.370016379345));
#21776=CARTESIAN_POINT('Ctrl Pts',(240.584720718821,156.909371480944,245.179908713947));
#21777=CARTESIAN_POINT('Ctrl Pts',(240.711375508263,156.862810604652,244.914832446015));
#21778=CARTESIAN_POINT('Ctrl Pts',(240.763953172911,156.842724194531,244.829821228398));
#21779=CARTESIAN_POINT('Ctrl Pts',(240.857506848798,156.803776862828,244.707325709514));
#21780=CARTESIAN_POINT('Ctrl Pts',(240.891134475151,156.789317054963,244.667330754476));
#21781=CARTESIAN_POINT('Ctrl Pts',(240.963066033618,156.757027041863,244.58901461358));
#21782=CARTESIAN_POINT('Ctrl Pts',(241.002349559882,156.738719066925,244.549787659307));
#21783=CARTESIAN_POINT('Ctrl Pts',(241.358027470615,156.565316622201,244.220670026599));
#21784=CARTESIAN_POINT('Ctrl Pts',(241.709462908565,156.342949227238,244.074128067476));
#21785=CARTESIAN_POINT('Ctrl Pts',(242.04928006672,156.018938485126,244.073593133703));
#21786=CARTESIAN_POINT('Ctrl Pts',(236.528689297355,150.229030128645,247.073589199254));
#21787=CARTESIAN_POINT('Ctrl Pts',(236.698998928806,150.066639190825,247.073269716825));
#21788=CARTESIAN_POINT('Ctrl Pts',(236.872669356512,149.92966652065,247.036390577158));
#21789=CARTESIAN_POINT('Ctrl Pts',(237.127746428412,149.756549620958,246.926232368273));
#21790=CARTESIAN_POINT('Ctrl Pts',(237.21190246902,149.704215227193,246.880373048748));
#21791=CARTESIAN_POINT('Ctrl Pts',(237.335824368256,149.632932480362,246.797874194614));
#21792=CARTESIAN_POINT('Ctrl Pts',(237.376748308819,149.610374208359,246.768089597428));
#21793=CARTESIAN_POINT('Ctrl Pts',(237.457684600991,149.567519259982,246.703950444775));
#21794=CARTESIAN_POINT('Ctrl Pts',(237.496910490698,149.547605679369,246.670325582074));
#21795=CARTESIAN_POINT('Ctrl Pts',(237.698299988104,149.449498601363,246.483479342273));
#21796=CARTESIAN_POINT('Ctrl Pts',(237.823942114196,149.400852263453,246.320448669587));
#21797=CARTESIAN_POINT('Ctrl Pts',(237.992420893058,149.338884077992,245.967279962524));
#21798=CARTESIAN_POINT('Ctrl Pts',(238.03544226452,149.325479801998,245.776985842833));
#21799=CARTESIAN_POINT('Ctrl Pts',(238.036014742284,149.325290926997,245.369914584485));
#21800=CARTESIAN_POINT('Ctrl Pts',(237.993179236838,149.338619575289,245.179793889859));
#21801=CARTESIAN_POINT('Ctrl Pts',(237.866527219159,149.385181894555,244.914735249744));
#21802=CARTESIAN_POINT('Ctrl Pts',(237.813956192467,149.405266919668,244.829736103342));
#21803=CARTESIAN_POINT('Ctrl Pts',(237.720420540777,149.444208076534,244.707267984196));
#21804=CARTESIAN_POINT('Ctrl Pts',(237.686800262615,149.458665134707,244.667283711223));
#21805=CARTESIAN_POINT('Ctrl Pts',(237.614885931005,149.490947953181,244.588992032097));
#21806=CARTESIAN_POINT('Ctrl Pts',(237.57558597426,149.509264161755,244.54975425391));
#21807=CARTESIAN_POINT('Ctrl Pts',(237.220147950135,149.682550133189,244.220906926231));
#21808=CARTESIAN_POINT('Ctrl Pts',(236.86867264184,149.904857581276,244.074366090943));
#21809=CARTESIAN_POINT('Ctrl Pts',(236.528686026679,150.229029898191,244.073593133703));
#21810=CARTESIAN_POINT('Origin',(239.288983046699,153.123984191658,271.473593133703));
#21811=CARTESIAN_POINT('',(242.463324619723,156.453181629146,272.073593133703));
#21812=CARTESIAN_POINT('Origin',(239.288983046699,153.123984191658,272.073593133703));
#21813=CARTESIAN_POINT('Origin',(242.463324619723,156.453181629146,271.473593133703));
#21814=CARTESIAN_POINT('Origin',(239.288983046699,153.123984191658,275.073593133703));
#21815=CARTESIAN_POINT('',(234.458463261663,148.05781417809,274.073593133703));
#21816=CARTESIAN_POINT('',(244.119502831735,158.190154205226,274.073593133703));
#21817=CARTESIAN_POINT('Origin',(239.288983046699,153.123984191658,274.073593133703));
#21818=CARTESIAN_POINT('Origin',(239.288983046699,153.123984191658,274.073593133703));
#21819=CARTESIAN_POINT('',(244.119502831735,158.190154205226,272.073593133703));
#21820=CARTESIAN_POINT('',(244.119502831735,158.190154205226,275.073593133703));
#21821=CARTESIAN_POINT('Origin',(239.288983046699,153.123984191658,272.073593133703));
#21822=CARTESIAN_POINT('Origin',(239.288983046699,153.123984191658,275.073593133703));
#21823=CARTESIAN_POINT('',(235.148537516668,148.781552751457,275.073593133703));
#21824=CARTESIAN_POINT('',(235.148537516668,148.781552751457,275.073593133703));
#21825=CARTESIAN_POINT('Origin',(239.288983046699,153.123984191658,275.073593133703));
#21826=CARTESIAN_POINT('Origin',(239.288983046699,153.123984191658,275.073593133703));
#21827=CARTESIAN_POINT('Origin',(244.355153060267,148.293464406622,272.073593133703));
#21828=CARTESIAN_POINT('Origin',(241.348236019854,151.160516285414,242.073593133703));
#21829=CARTESIAN_POINT('Ctrl Pts',(236.873740135465,150.590916994567,244.573617786368));
#21830=CARTESIAN_POINT('Ctrl Pts',(237.067896863957,150.406853907471,244.57412083749));
#21831=CARTESIAN_POINT('Ctrl Pts',(237.306162889608,150.283920204409,244.68441000503));
#21832=CARTESIAN_POINT('Ctrl Pts',(237.692910780473,150.159951448154,245.049509635926));
#21833=CARTESIAN_POINT('Ctrl Pts',(237.83095860781,150.145218109284,245.307954643826));
#21834=CARTESIAN_POINT('Ctrl Pts',(237.830050941306,150.145357961667,245.840602772399));
#21835=CARTESIAN_POINT('Ctrl Pts',(237.69255105899,150.160009424731,246.097805133848));
#21836=CARTESIAN_POINT('Ctrl Pts',(237.305689220764,150.284135029502,246.463439756173));
#21837=CARTESIAN_POINT('Ctrl Pts',(237.066826432402,150.407492962315,246.573505429044));
#21838=CARTESIAN_POINT('Ctrl Pts',(236.67849369465,150.776402672902,246.573629303778));
#21839=CARTESIAN_POINT('Ctrl Pts',(236.546110415943,151.008822191958,246.462786768509));
#21840=CARTESIAN_POINT('Ctrl Pts',(236.404533343642,151.388433385931,246.097308333644));
#21841=CARTESIAN_POINT('Ctrl Pts',(236.382970368025,151.525881299787,245.838716869155));
#21842=CARTESIAN_POINT('Ctrl Pts',(236.383187759016,151.524892706649,245.306031962191));
#21843=CARTESIAN_POINT('Ctrl Pts',(236.404742516748,151.387822200401,245.049123050581));
#21844=CARTESIAN_POINT('Ctrl Pts',(236.546338451014,151.008285431764,244.684044657033));
#21845=CARTESIAN_POINT('Ctrl Pts',(236.679583406974,150.774980081663,244.573114735247));
#21846=CARTESIAN_POINT('Ctrl Pts',(236.873740135465,150.590916994567,244.573617786368));
#21847=CARTESIAN_POINT('Ctrl Pts',(236.525220476937,150.225395286397,244.068571160446));
#21848=CARTESIAN_POINT('Ctrl Pts',(236.859135544773,149.908227964641,244.069328280267));
#21849=CARTESIAN_POINT('Ctrl Pts',(237.239285345497,149.66505329898,244.235319896002));
#21850=CARTESIAN_POINT('Ctrl Pts',(237.834511238579,149.377627059051,244.784816607079));
#21851=CARTESIAN_POINT('Ctrl Pts',(238.038464934868,149.31692107592,245.173796444513));
#21852=CARTESIAN_POINT('Ctrl Pts',(238.03711156165,149.317381210123,245.975453482869));
#21853=CARTESIAN_POINT('Ctrl Pts',(237.833974075219,149.377813068345,246.36256311913));
#21854=CARTESIAN_POINT('Ctrl Pts',(237.238538243332,149.665494695115,246.912864913618));
#21855=CARTESIAN_POINT('Ctrl Pts',(236.857403792907,149.909442529541,247.078520196222));
#21856=CARTESIAN_POINT('Ctrl Pts',(236.189317857989,150.544896610707,247.07870666254));
#21857=CARTESIAN_POINT('Ctrl Pts',(235.930781024921,150.912925475016,246.91188217622));
#21858=CARTESIAN_POINT('Ctrl Pts',(235.616533387526,151.492474252108,246.36181535786));
#21859=CARTESIAN_POINT('Ctrl Pts',(235.545715512323,151.6937528812,245.972615210562));
#21860=CARTESIAN_POINT('Ctrl Pts',(235.546314987901,151.692287243042,245.170902571576));
#21861=CARTESIAN_POINT('Ctrl Pts',(235.61701217298,151.491546588432,244.784234780814));
#21862=CARTESIAN_POINT('Ctrl Pts',(235.931265658698,150.912097964328,244.234770018165));
#21863=CARTESIAN_POINT('Ctrl Pts',(236.1913054091,150.542562608153,244.067814040624));
#21864=CARTESIAN_POINT('Ctrl Pts',(236.525220476937,150.225395286397,244.068571160446));
#21865=CARTESIAN_POINT('Ctrl Pts',(241.704225957933,155.65705138875,244.573617786368));
#21866=CARTESIAN_POINT('Ctrl Pts',(241.510069229442,155.841114475846,244.57412083749));
#21867=CARTESIAN_POINT('Ctrl Pts',(241.27180320379,155.964048178908,244.68441000503));
#21868=CARTESIAN_POINT('Ctrl Pts',(240.885055312925,156.088016935163,245.049509635926));
#21869=CARTESIAN_POINT('Ctrl Pts',(240.747007485588,156.102750274032,245.307954643826));
#21870=CARTESIAN_POINT('Ctrl Pts',(240.747915152092,156.102610421649,245.840602772399));
#21871=CARTESIAN_POINT('Ctrl Pts',(240.885415034409,156.087958958585,246.097805133848));
#21872=CARTESIAN_POINT('Ctrl Pts',(241.272276872634,155.963833353815,246.463439756173));
#21873=CARTESIAN_POINT('Ctrl Pts',(241.511139660996,155.840475421002,246.573505429044));
#21874=CARTESIAN_POINT('Ctrl Pts',(241.899472398749,155.471565710415,246.573629303778));
#21875=CARTESIAN_POINT('Ctrl Pts',(242.031855677455,155.239146191359,246.462786768509));
#21876=CARTESIAN_POINT('Ctrl Pts',(242.173432749756,154.859534997386,246.097308333644));
#21877=CARTESIAN_POINT('Ctrl Pts',(242.194995725373,154.72208708353,245.838716869155));
#21878=CARTESIAN_POINT('Ctrl Pts',(242.194778334383,154.723075676668,245.306031962191));
#21879=CARTESIAN_POINT('Ctrl Pts',(242.17322357665,154.860146182915,245.049123050581));
#21880=CARTESIAN_POINT('Ctrl Pts',(242.031627642384,155.239682951552,244.684044657033));
#21881=CARTESIAN_POINT('Ctrl Pts',(241.898382686424,155.472988301653,244.573114735247));
#21882=CARTESIAN_POINT('Ctrl Pts',(241.704225957933,155.65705138875,244.573617786368));
#21883=CARTESIAN_POINT('Ctrl Pts',(242.052768019306,156.022596592656,244.068538696047));
#21884=CARTESIAN_POINT('Ctrl Pts',(241.718843967803,156.339772470352,244.0692958322));
#21885=CARTESIAN_POINT('Ctrl Pts',(241.33868504679,156.582954865103,244.235291028488));
#21886=CARTESIAN_POINT('Ctrl Pts',(240.743445752741,156.870391612079,244.78479959261));
#21887=CARTESIAN_POINT('Ctrl Pts',(240.539487820023,156.931100550332,245.173787820824));
#21888=CARTESIAN_POINT('Ctrl Pts',(240.540841221892,156.930640395541,245.975462151073));
#21889=CARTESIAN_POINT('Ctrl Pts',(240.743982927508,156.870205594555,246.362580137774));
#21890=CARTESIAN_POINT('Ctrl Pts',(241.339432166532,156.582513454404,246.912893802668));
#21891=CARTESIAN_POINT('Ctrl Pts',(241.720575762179,156.338557868458,247.078552658573));
#21892=CARTESIAN_POINT('Ctrl Pts',(242.388679679633,155.703086653819,247.078739128914));
#21893=CARTESIAN_POINT('Ctrl Pts',(242.647224621851,155.335049072542,246.911911044074));
#21894=CARTESIAN_POINT('Ctrl Pts',(242.961483358511,154.755487443462,246.361832360372));
#21895=CARTESIAN_POINT('Ctrl Pts',(243.032304399819,154.554204711331,245.972623817548));
#21896=CARTESIAN_POINT('Ctrl Pts',(243.031704899681,154.555670380153,245.170893885459));
#21897=CARTESIAN_POINT('Ctrl Pts',(242.961004555727,154.756415127481,244.784217753795));
#21898=CARTESIAN_POINT('Ctrl Pts',(242.646739971581,155.33587660192,244.234741138791));
#21899=CARTESIAN_POINT('Ctrl Pts',(242.386692070809,155.705420714959,244.067781559894));
#21900=CARTESIAN_POINT('Ctrl Pts',(242.052768019306,156.022596592656,244.068538696047));
#21901=CARTESIAN_POINT('Ctrl Pts',(272.893594663547,160.159358297364,244.573616253716));
#21902=CARTESIAN_POINT('Ctrl Pts',(273.160746650237,160.173717428468,244.574119305608));
#21903=CARTESIAN_POINT('Ctrl Pts',(273.413857808985,160.262139317963,244.684408642187));
#21904=CARTESIAN_POINT('Ctrl Pts',(273.76983864822,160.457639798944,245.049508832668));
#21905=CARTESIAN_POINT('Ctrl Pts',(273.875476617283,160.547722831363,245.3079542367));
#21906=CARTESIAN_POINT('Ctrl Pts',(273.874750844349,160.547160093815,245.840603181627));
#21907=CARTESIAN_POINT('Ctrl Pts',(273.769549161884,160.45741853231,246.097805937303));
#21908=CARTESIAN_POINT('Ctrl Pts',(273.413376091047,160.261943203446,246.463441120033));
#21909=CARTESIAN_POINT('Ctrl Pts',(273.159546539055,160.173379857016,246.5735069616));
#21910=CARTESIAN_POINT('Ctrl Pts',(272.624660495995,160.145186473407,246.573630836524));
#21911=CARTESIAN_POINT('Ctrl Pts',(272.364888729948,160.208928826216,246.462788131368));
#21912=CARTESIAN_POINT('Ctrl Pts',(271.991939938556,160.367227701822,246.097309136337));
#21913=CARTESIAN_POINT('Ctrl Pts',(271.877329515132,160.446103563013,245.838717275493));
#21914=CARTESIAN_POINT('Ctrl Pts',(271.878196696175,160.445581475241,245.306031552117));
#21915=CARTESIAN_POINT('Ctrl Pts',(271.992527488176,160.36695920955,245.049122246731));
#21916=CARTESIAN_POINT('Ctrl Pts',(272.365435222693,160.208725212658,244.68404329363));
#21917=CARTESIAN_POINT('Ctrl Pts',(272.626442676856,160.14499916626,244.573113201823));
#21918=CARTESIAN_POINT('Ctrl Pts',(272.893594663547,160.159358297364,244.573616253716));
#21919=CARTESIAN_POINT('Ctrl Pts',(272.919178153013,159.656406407913,244.070014088572));
#21920=CARTESIAN_POINT('Ctrl Pts',(273.378524344086,159.680652607522,244.070770482515));
#21921=CARTESIAN_POINT('Ctrl Pts',(273.815975906659,159.789321495117,244.236602955261));
#21922=CARTESIAN_POINT('Ctrl Pts',(274.433249479638,160.023637725035,244.785572840259));
#21923=CARTESIAN_POINT('Ctrl Pts',(274.617362800752,160.129901128078,245.174179737123));
#21924=CARTESIAN_POINT('Ctrl Pts',(274.616099527232,160.129235398268,245.975068211741));
#21925=CARTESIAN_POINT('Ctrl Pts',(274.432745627596,160.023375815266,246.361806700368));
#21926=CARTESIAN_POINT('Ctrl Pts',(273.815142664649,159.789082827464,246.911580897118));
#21927=CARTESIAN_POINT('Ctrl Pts',(273.376454115703,159.680230997393,247.077077359117));
#21928=CARTESIAN_POINT('Ctrl Pts',(272.456774314034,159.632322621868,247.077263646609));
#21929=CARTESIAN_POINT('Ctrl Pts',(272.012324858108,159.697744007317,246.910599101822));
#21930=CARTESIAN_POINT('Ctrl Pts',(271.376232398275,159.868164538219,246.361059656098));
#21931=CARTESIAN_POINT('Ctrl Pts',(271.181638548661,159.955159945194,245.972232660372));
#21932=CARTESIAN_POINT('Ctrl Pts',(271.183113076211,159.95458729014,245.171288638899));
#21933=CARTESIAN_POINT('Ctrl Pts',(271.377233932998,159.86787417663,244.784991571802));
#21934=CARTESIAN_POINT('Ctrl Pts',(272.013257787885,159.697526747734,244.23605360463));
#21935=CARTESIAN_POINT('Ctrl Pts',(272.45983196194,159.632160208303,244.06925769463));
#21936=CARTESIAN_POINT('Ctrl Pts',(272.919178153013,159.656406407913,244.070014088572));
#21937=CARTESIAN_POINT('',(272.893595756463,160.159336843574,246.573593133381));
#21938=CARTESIAN_POINT('',(272.893595838066,160.159335207205,244.573593133703));
#21939=CARTESIAN_POINT('Ctrl Pts',(272.89359575648,160.159336843253,246.573593133703));
#21940=CARTESIAN_POINT('Ctrl Pts',(272.84861813654,160.156998423751,246.573593133777));
#21941=CARTESIAN_POINT('Ctrl Pts',(272.803777913346,160.156762969772,246.570551147));
#21942=CARTESIAN_POINT('Ctrl Pts',(272.715012383882,160.160063357393,246.558577698866));
#21943=CARTESIAN_POINT('Ctrl Pts',(272.671223817618,160.16358947227,246.549670593028));
#21944=CARTESIAN_POINT('Ctrl Pts',(272.54162313439,160.179134800402,246.514389597396));
#21945=CARTESIAN_POINT('Ctrl Pts',(272.459292925889,160.196044952057,246.47971112174));
#21946=CARTESIAN_POINT('Ctrl Pts',(272.331884596952,160.231139310487,246.405940491082));
#21947=CARTESIAN_POINT('Ctrl Pts',(272.283580104659,160.247054870222,246.372086195779));
#21948=CARTESIAN_POINT('Ctrl Pts',(272.212830121178,160.273690718174,246.313003139576));
#21949=CARTESIAN_POINT('Ctrl Pts',(272.188116124322,160.283827212976,246.290206730023));
#21950=CARTESIAN_POINT('Ctrl Pts',(272.141019691395,160.304086208312,246.242334167609));
#21951=CARTESIAN_POINT('Ctrl Pts',(272.118425274288,160.314223541269,246.216956137048));
#21952=CARTESIAN_POINT('Ctrl Pts',(272.057113716637,160.342801676355,246.140681005568));
#21953=CARTESIAN_POINT('Ctrl Pts',(272.021679560313,160.360726146822,246.086958711194));
#21954=CARTESIAN_POINT('Ctrl Pts',(271.96416665625,160.391729751442,245.978032102337));
#21955=CARTESIAN_POINT('Ctrl Pts',(271.941189971409,160.405090586035,245.923416774258));
#21956=CARTESIAN_POINT('Ctrl Pts',(271.893378613539,160.43433731398,245.772513348258));
#21957=CARTESIAN_POINT('Ctrl Pts',(271.877672652427,160.445890623876,245.673483077983));
#21958=CARTESIAN_POINT('Ctrl Pts',(271.877787775074,160.445750590394,245.473008288347));
#21959=CARTESIAN_POINT('Ctrl Pts',(271.893469585958,160.434311803733,245.374193081088));
#21960=CARTESIAN_POINT('Ctrl Pts',(271.941368526616,160.405077356024,245.223303692942));
#21961=CARTESIAN_POINT('Ctrl Pts',(271.964343198474,160.391727578948,245.168765169821));
#21962=CARTESIAN_POINT('Ctrl Pts',(272.021861156968,160.36070465498,245.059926304005));
#21963=CARTESIAN_POINT('Ctrl Pts',(272.057309400142,160.342745164453,245.006226072545));
#21964=CARTESIAN_POINT('Ctrl Pts',(272.118660575559,160.314122358304,244.929954836604));
#21965=CARTESIAN_POINT('Ctrl Pts',(272.141286933469,160.303965616176,244.904560232997));
#21966=CARTESIAN_POINT('Ctrl Pts',(272.188411027287,160.283707825989,244.856699719665));
#21967=CARTESIAN_POINT('Ctrl Pts',(272.213087436914,160.273595046995,244.833955999993));
#21968=CARTESIAN_POINT('Ctrl Pts',(272.283776953734,160.246980411639,244.774957037283));
#21969=CARTESIAN_POINT('Ctrl Pts',(272.332054369033,160.23106401385,244.741137633888));
#21970=CARTESIAN_POINT('Ctrl Pts',(272.459465282786,160.195958053628,244.667392469805));
#21971=CARTESIAN_POINT('Ctrl Pts',(272.541825403793,160.179055115833,244.632719291294));
#21972=CARTESIAN_POINT('Ctrl Pts',(272.67145705261,160.16354874035,244.597463836825));
#21973=CARTESIAN_POINT('Ctrl Pts',(272.715232192116,160.160039330037,244.588569745954));
#21974=CARTESIAN_POINT('Ctrl Pts',(272.803922751181,160.156765637209,244.576624852807));
#21975=CARTESIAN_POINT('Ctrl Pts',(272.848689914664,160.157006237089,244.573593133703));
#21976=CARTESIAN_POINT('Ctrl Pts',(272.893595838066,160.159335207205,244.573593133703));
#21977=CARTESIAN_POINT('',(272.918996157899,159.659984078124,247.073589514835));
#21978=CARTESIAN_POINT('',(272.893595648979,160.159338953007,246.573591021215));
#21979=CARTESIAN_POINT('',(272.918996332872,159.659980853205,244.073593137428));
#21980=CARTESIAN_POINT('Ctrl Pts',(272.918996332834,159.659980853954,244.073593133703));
#21981=CARTESIAN_POINT('Ctrl Pts',(272.684677113858,159.648061814786,244.073325863255));
#21982=CARTESIAN_POINT('Ctrl Pts',(272.464124179613,159.657462336297,244.109847139091));
#21983=CARTESIAN_POINT('Ctrl Pts',(272.158086920106,159.692555569418,244.219811905837));
#21984=CARTESIAN_POINT('Ctrl Pts',(272.060168313579,159.70775995013,244.265663970251));
#21985=CARTESIAN_POINT('Ctrl Pts',(271.872812989298,159.743488842164,244.37576238341));
#21986=CARTESIAN_POINT('Ctrl Pts',(271.784976843385,159.763591097843,244.438626167558));
#21987=CARTESIAN_POINT('Ctrl Pts',(271.524682254253,159.832061411953,244.663127176969));
#21988=CARTESIAN_POINT('Ctrl Pts',(271.397541667612,159.877211097541,244.826245103114));
#21989=CARTESIAN_POINT('Ctrl Pts',(271.229134999604,159.940259016219,245.17938212848));
#21990=CARTESIAN_POINT('Ctrl Pts',(271.187673154397,159.958215997785,245.369501892319));
#21991=CARTESIAN_POINT('Ctrl Pts',(271.186957902735,159.958511753159,245.776239362339));
#21992=CARTESIAN_POINT('Ctrl Pts',(271.228127696939,159.940658438962,245.966395214971));
#21993=CARTESIAN_POINT('Ctrl Pts',(271.354646900259,159.893259013043,246.231809670352));
#21994=CARTESIAN_POINT('Ctrl Pts',(271.407668107912,159.87415637492,246.316977934885));
#21995=CARTESIAN_POINT('Ctrl Pts',(271.504112506007,159.842601973052,246.439775500791));
#21996=CARTESIAN_POINT('Ctrl Pts',(271.539080824339,159.831609459822,246.479882217612));
#21997=CARTESIAN_POINT('Ctrl Pts',(271.614770265428,159.809128983085,246.558444040955));
#21998=CARTESIAN_POINT('Ctrl Pts',(271.656587198068,159.797353514779,246.597842459808));
#21999=CARTESIAN_POINT('Ctrl Pts',(272.039253889,159.696787821332,246.927734975046));
#22000=CARTESIAN_POINT('Ctrl Pts',(272.44884461053,159.636065800518,247.074098313406));
#22001=CARTESIAN_POINT('Ctrl Pts',(272.918996199032,159.659983271947,247.073589666413));
#22002=CARTESIAN_POINT('',(272.893595838066,160.159335207205,244.573593133703));
#22003=CARTESIAN_POINT('Ctrl Pts',(272.537990049465,167.150273777714,244.573616253716));
#22004=CARTESIAN_POINT('Ctrl Pts',(272.270838062775,167.13591464661,244.574119305608));
#22005=CARTESIAN_POINT('Ctrl Pts',(272.017726904027,167.047492757115,244.684408642187));
#22006=CARTESIAN_POINT('Ctrl Pts',(271.661746064792,166.851992276134,245.049508832668));
#22007=CARTESIAN_POINT('Ctrl Pts',(271.556108095729,166.761909243715,245.3079542367));
#22008=CARTESIAN_POINT('Ctrl Pts',(271.556833868663,166.762471981263,245.840603181627));
#22009=CARTESIAN_POINT('Ctrl Pts',(271.662035551128,166.852213542768,246.097805937303));
#22010=CARTESIAN_POINT('Ctrl Pts',(272.018208621965,167.047688871632,246.463441120033));
#22011=CARTESIAN_POINT('Ctrl Pts',(272.272038173957,167.136252218062,246.5735069616));
#22012=CARTESIAN_POINT('Ctrl Pts',(272.806924217017,167.164445601671,246.573630836524));
#22013=CARTESIAN_POINT('Ctrl Pts',(273.066695983064,167.100703248862,246.462788131368));
#22014=CARTESIAN_POINT('Ctrl Pts',(273.439644774456,166.942404373256,246.097309136337));
#22015=CARTESIAN_POINT('Ctrl Pts',(273.55425519788,166.863528512065,245.838717275493));
#22016=CARTESIAN_POINT('Ctrl Pts',(273.553388016837,166.864050599837,245.306031552117));
#22017=CARTESIAN_POINT('Ctrl Pts',(273.439057224836,166.942672865528,245.049122246731));
#22018=CARTESIAN_POINT('Ctrl Pts',(273.066149490319,167.10090686242,244.68404329363));
#22019=CARTESIAN_POINT('Ctrl Pts',(272.805142036156,167.164632908818,244.573113201823));
#22020=CARTESIAN_POINT('Ctrl Pts',(272.537990049465,167.150273777714,244.573616253716));
#22021=CARTESIAN_POINT('Ctrl Pts',(272.512403161391,167.65329248121,244.069947188143));
#22022=CARTESIAN_POINT('Ctrl Pts',(272.053031438508,167.629044968165,244.07070361574));
#22023=CARTESIAN_POINT('Ctrl Pts',(271.615555387453,167.520373390882,244.236543467048));
#22024=CARTESIAN_POINT('Ctrl Pts',(270.998247103352,167.286052004531,244.785537777997));
#22025=CARTESIAN_POINT('Ctrl Pts',(270.814123357274,167.179786452026,245.174161966009));
#22026=CARTESIAN_POINT('Ctrl Pts',(270.815386702198,167.180452195518,245.975086074588));
#22027=CARTESIAN_POINT('Ctrl Pts',(270.998750983871,167.2863139197,246.361841771234));
#22028=CARTESIAN_POINT('Ctrl Pts',(271.616388676161,167.520612064187,246.911640429713));
#22029=CARTESIAN_POINT('Ctrl Pts',(272.05510178248,167.629466589457,247.077144255326));
#22030=CARTESIAN_POINT('Ctrl Pts',(272.974832701618,167.677377583998,247.07733055111));
#22031=CARTESIAN_POINT('Ctrl Pts',(273.419306690832,167.611955975499,246.910658590737));
#22032=CARTESIAN_POINT('Ctrl Pts',(274.055434107672,167.44153383431,246.361094693722));
#22033=CARTESIAN_POINT('Ctrl Pts',(274.250038582589,167.354537348704,245.972250397064));
#22034=CARTESIAN_POINT('Ctrl Pts',(274.248563974356,167.355110010476,245.171270739137));
#22035=CARTESIAN_POINT('Ctrl Pts',(274.054432517953,167.441824198804,244.784956483677));
#22036=CARTESIAN_POINT('Ctrl Pts',(273.418373709719,167.612173236895,244.235994091974));
#22037=CARTESIAN_POINT('Ctrl Pts',(272.971774884274,167.677539994255,244.069190760545));
#22038=CARTESIAN_POINT('Ctrl Pts',(272.512403161391,167.65329248121,244.069947188143));
#22039=CARTESIAN_POINT('',(272.53798895654,167.150295231503,246.573593133381));
#22040=CARTESIAN_POINT('',(272.537988874946,167.150296867873,244.573593133703));
#22041=CARTESIAN_POINT('Ctrl Pts',(272.537988956523,167.150295231825,246.573593133703));
#22042=CARTESIAN_POINT('Ctrl Pts',(272.582966576466,167.152633651326,246.573593133777));
#22043=CARTESIAN_POINT('Ctrl Pts',(272.627806799662,167.152869105306,246.570551147));
#22044=CARTESIAN_POINT('Ctrl Pts',(272.716572329129,167.149568717685,246.558577698866));
#22045=CARTESIAN_POINT('Ctrl Pts',(272.760360895393,167.146042602808,246.549670593028));
#22046=CARTESIAN_POINT('Ctrl Pts',(272.889961578622,167.130497274676,246.514389597396));
#22047=CARTESIAN_POINT('Ctrl Pts',(272.972291787123,167.113587123021,246.47971112174));
#22048=CARTESIAN_POINT('Ctrl Pts',(273.09970011606,167.078492764591,246.405940491082));
#22049=CARTESIAN_POINT('Ctrl Pts',(273.148004608353,167.062577204855,246.372086195779));
#22050=CARTESIAN_POINT('Ctrl Pts',(273.218754591834,167.035941356904,246.313003139576));
#22051=CARTESIAN_POINT('Ctrl Pts',(273.24346858869,167.025804862102,246.290206730023));
#22052=CARTESIAN_POINT('Ctrl Pts',(273.290565021617,167.005545866766,246.242334167609));
#22053=CARTESIAN_POINT('Ctrl Pts',(273.313159438724,166.995408533809,246.216956137048));
#22054=CARTESIAN_POINT('Ctrl Pts',(273.374470996374,166.966830398723,246.140681005568));
#22055=CARTESIAN_POINT('Ctrl Pts',(273.409905152699,166.948905928256,246.086958711195));
#22056=CARTESIAN_POINT('Ctrl Pts',(273.467418056762,166.917902323636,245.978032102338));
#22057=CARTESIAN_POINT('Ctrl Pts',(273.490394741603,166.904541489043,245.923416774259));
#22058=CARTESIAN_POINT('Ctrl Pts',(273.538206099473,166.875294761098,245.772513348258));
#22059=CARTESIAN_POINT('Ctrl Pts',(273.553912060585,166.863741451202,245.673483077984));
#22060=CARTESIAN_POINT('Ctrl Pts',(273.553796937938,166.863881484684,245.473008288348));
#22061=CARTESIAN_POINT('Ctrl Pts',(273.538115127054,166.875320271345,245.374193081089));
#22062=CARTESIAN_POINT('Ctrl Pts',(273.490216186397,166.904554719054,245.223303692942));
#22063=CARTESIAN_POINT('Ctrl Pts',(273.467241514539,166.91790449613,245.168765169821));
#22064=CARTESIAN_POINT('Ctrl Pts',(273.409723556044,166.948927420098,245.059926304005));
#22065=CARTESIAN_POINT('Ctrl Pts',(273.37427531287,166.966886910625,245.006226072545));
#22066=CARTESIAN_POINT('Ctrl Pts',(273.312924137453,166.995509716774,244.929954836604));
#22067=CARTESIAN_POINT('Ctrl Pts',(273.290297779544,167.005666458902,244.904560232997));
#22068=CARTESIAN_POINT('Ctrl Pts',(273.243173685724,167.02592424909,244.856699719664));
#22069=CARTESIAN_POINT('Ctrl Pts',(273.218497276097,167.036037028083,244.833955999992));
#22070=CARTESIAN_POINT('Ctrl Pts',(273.147807759279,167.062651663438,244.774957037284));
#22071=CARTESIAN_POINT('Ctrl Pts',(273.099530343979,167.078568061228,244.741137633888));
#22072=CARTESIAN_POINT('Ctrl Pts',(272.972119430226,167.11367402145,244.667392469805));
#22073=CARTESIAN_POINT('Ctrl Pts',(272.889759309219,167.130576959245,244.632719291294));
#22074=CARTESIAN_POINT('Ctrl Pts',(272.760127660401,167.146083334728,244.597463836825));
#22075=CARTESIAN_POINT('Ctrl Pts',(272.716352520896,167.149592745041,244.588569745954));
#22076=CARTESIAN_POINT('Ctrl Pts',(272.627661961831,167.152866437869,244.576624852807));
#22077=CARTESIAN_POINT('Ctrl Pts',(272.582894798349,167.152625837989,244.573593133703));
#22078=CARTESIAN_POINT('Ctrl Pts',(272.537988874946,167.150296867873,244.573593133703));
#22079=CARTESIAN_POINT('',(272.512586339276,167.649647881398,247.073589202258));
#22080=CARTESIAN_POINT('',(272.537989064033,167.150293122071,246.573591021215));
#22081=CARTESIAN_POINT('',(272.51258838014,167.649651221873,244.073593137428));
#22082=CARTESIAN_POINT('Ctrl Pts',(272.512588380178,167.649651221123,244.073593133703));
#22083=CARTESIAN_POINT('Ctrl Pts',(272.746773917338,167.661563460343,244.073207336743));
#22084=CARTESIAN_POINT('Ctrl Pts',(272.967263075997,167.652182489951,244.109671982816));
#22085=CARTESIAN_POINT('Ctrl Pts',(273.273311423625,167.617102815298,244.219644650044));
#22086=CARTESIAN_POINT('Ctrl Pts',(273.371251311414,167.6019004664,244.26551482214));
#22087=CARTESIAN_POINT('Ctrl Pts',(273.558682837338,167.566163320439,244.375680399037));
#22088=CARTESIAN_POINT('Ctrl Pts',(273.646645002999,167.546032094573,244.438654405421));
#22089=CARTESIAN_POINT('Ctrl Pts',(273.906938958271,167.477559290898,244.663166238249));
#22090=CARTESIAN_POINT('Ctrl Pts',(274.034076078324,167.432409299256,244.826292334005));
#22091=CARTESIAN_POINT('Ctrl Pts',(274.202470426655,167.369364615484,245.179447606592));
#22092=CARTESIAN_POINT('Ctrl Pts',(274.243923553764,167.351411117335,245.369584971744));
#22093=CARTESIAN_POINT('Ctrl Pts',(274.244615114457,167.351125158105,245.776329368437));
#22094=CARTESIAN_POINT('Ctrl Pts',(274.203430535256,167.368984709093,245.966487747264));
#22095=CARTESIAN_POINT('Ctrl Pts',(274.076883746714,167.416392740919,246.231904586228));
#22096=CARTESIAN_POINT('Ctrl Pts',(274.023852437588,167.43549810258,246.317073411003));
#22097=CARTESIAN_POINT('Ctrl Pts',(273.927391417782,167.467055829036,246.439871465846));
#22098=CARTESIAN_POINT('Ctrl Pts',(273.892417314405,167.478049322204,246.479978287074));
#22099=CARTESIAN_POINT('Ctrl Pts',(273.816715804945,167.500531393776,246.55854020209));
#22100=CARTESIAN_POINT('Ctrl Pts',(273.774892281931,167.512307489834,246.597938651966));
#22101=CARTESIAN_POINT('Ctrl Pts',(273.39219560437,167.612869582687,246.927807707392));
#22102=CARTESIAN_POINT('Ctrl Pts',(272.983080973498,167.673583875118,247.074228761836));
#22103=CARTESIAN_POINT('Ctrl Pts',(272.512586298077,167.649648688282,247.073589199254));
#22104=CARTESIAN_POINT('',(272.537988874946,167.150296867873,244.573593133703));
#22105=CARTESIAN_POINT('Origin',(272.918996332834,159.659980853954,245.573593133703));
#22106=CARTESIAN_POINT('Ctrl Pts',(272.893595838066,160.159335207205,244.573593133703));
#22107=CARTESIAN_POINT('Ctrl Pts',(272.994616473054,160.164574472366,244.573593133703));
#22108=CARTESIAN_POINT('Ctrl Pts',(273.093662374227,160.180056064334,244.588926668372));
#22109=CARTESIAN_POINT('Ctrl Pts',(273.219128553104,160.210726797024,244.628234491494));
#22110=CARTESIAN_POINT('Ctrl Pts',(273.249831367943,160.219204367691,244.639604524938));
#22111=CARTESIAN_POINT('Ctrl Pts',(273.407689912623,160.26748834392,244.707242077007));
#22112=CARTESIAN_POINT('Ctrl Pts',(273.51238388592,160.315968713744,244.784746950619));
#22113=CARTESIAN_POINT('Ctrl Pts',(273.605317555611,160.367292821967,244.880838247272));
#22114=CARTESIAN_POINT('Ctrl Pts',(273.616512492842,160.373584974036,244.89301514354));
#22115=CARTESIAN_POINT('Ctrl Pts',(273.638351446563,160.386067565299,244.918011816566));
#22116=CARTESIAN_POINT('Ctrl Pts',(273.648992741935,160.392257403739,244.930834103936));
#22117=CARTESIAN_POINT('Ctrl Pts',(273.698212284866,160.421369893916,244.993308664964));
#22118=CARTESIAN_POINT('Ctrl Pts',(273.732636125182,160.443230582208,245.046721221241));
#22119=CARTESIAN_POINT('Ctrl Pts',(273.788644179573,160.480856811058,245.155343526424));
#22120=CARTESIAN_POINT('Ctrl Pts',(273.811078606603,160.496980228528,245.209956194151));
#22121=CARTESIAN_POINT('Ctrl Pts',(273.844618130314,160.522223407935,245.317836348554));
#22122=CARTESIAN_POINT('Ctrl Pts',(273.856602086653,160.531853954495,245.37057049282));
#22123=CARTESIAN_POINT('Ctrl Pts',(273.871541519234,160.544235433038,245.473637636457));
#22124=CARTESIAN_POINT('Ctrl Pts',(273.875146524561,160.547467285949,245.523509871061));
#22125=CARTESIAN_POINT('Ctrl Pts',(273.875152125532,160.547339455183,245.66744290748));
#22126=CARTESIAN_POINT('Ctrl Pts',(273.862589234204,160.535782206681,245.766443228677));
#22127=CARTESIAN_POINT('Ctrl Pts',(273.816003541422,160.500425343,245.923804651633));
#22128=CARTESIAN_POINT('Ctrl Pts',(273.794496765221,160.48482593628,245.978365805299));
#22129=CARTESIAN_POINT('Ctrl Pts',(273.74041500634,160.448146636058,246.087229534119));
#22130=CARTESIAN_POINT('Ctrl Pts',(273.706974062563,160.426691435871,246.14092965317));
#22131=CARTESIAN_POINT('Ctrl Pts',(273.648845164208,160.391985299248,246.21720597302));
#22132=CARTESIAN_POINT('Ctrl Pts',(273.627363573115,160.379578351121,246.242605470456));
#22133=CARTESIAN_POINT('Ctrl Pts',(273.582546114185,160.354632982326,246.290460601382));
#22134=CARTESIAN_POINT('Ctrl Pts',(273.55901778022,160.342061412841,246.313212577002));
#22135=CARTESIAN_POINT('Ctrl Pts',(273.491409518233,160.308447258061,246.372197845411));
#22136=CARTESIAN_POINT('Ctrl Pts',(273.445024697867,160.287769251785,246.406000105603));
#22137=CARTESIAN_POINT('Ctrl Pts',(273.358606430672,160.254271830567,246.457744032174));
#22138=CARTESIAN_POINT('Ctrl Pts',(273.319995253228,160.240805734068,246.477508148981));
#22139=CARTESIAN_POINT('Ctrl Pts',(273.249957547624,160.219355296728,246.507530839586));
#22140=CARTESIAN_POINT('Ctrl Pts',(273.219244688596,160.210860905962,246.518909668632));
#22141=CARTESIAN_POINT('Ctrl Pts',(273.093736058858,160.180122398011,246.558247879177));
#22142=CARTESIAN_POINT('Ctrl Pts',(272.994663057878,160.164591406496,246.573593133538));
#22143=CARTESIAN_POINT('Ctrl Pts',(272.89359575648,160.159336843253,246.573593133703));
#22144=CARTESIAN_POINT('',(272.918996332834,159.659980853954,246.573593133703));
#22145=CARTESIAN_POINT('Ctrl Pts',(272.537988874946,167.150296867873,244.573593133703));
#22146=CARTESIAN_POINT('Ctrl Pts',(272.436968239958,167.145057602712,244.573593133703));
#22147=CARTESIAN_POINT('Ctrl Pts',(272.337922338785,167.129576010743,244.588926668372));
#22148=CARTESIAN_POINT('Ctrl Pts',(272.212456159909,167.098905278054,244.628234491494));
#22149=CARTESIAN_POINT('Ctrl Pts',(272.18175334507,167.090427707387,244.639604524937));
#22150=CARTESIAN_POINT('Ctrl Pts',(272.023894800388,167.042143731157,244.707242077008));
#22151=CARTESIAN_POINT('Ctrl Pts',(271.919200827091,166.993663361333,244.78474695062));
#22152=CARTESIAN_POINT('Ctrl Pts',(271.826267157402,166.942339253112,244.880838247271));
#22153=CARTESIAN_POINT('Ctrl Pts',(271.81507222017,166.936047101043,244.893015143539));
#22154=CARTESIAN_POINT('Ctrl Pts',(271.793233266447,166.923564509778,244.918011816568));
#22155=CARTESIAN_POINT('Ctrl Pts',(271.782591971076,166.917374671339,244.930834103937));
#22156=CARTESIAN_POINT('Ctrl Pts',(271.733372428147,166.888262181162,244.993308664963));
#22157=CARTESIAN_POINT('Ctrl Pts',(271.69894858783,166.86640149287,245.046721221241));
#22158=CARTESIAN_POINT('Ctrl Pts',(271.642940533439,166.82877526402,245.155343526424));
#22159=CARTESIAN_POINT('Ctrl Pts',(271.620506106409,166.81265184655,245.209956194151));
#22160=CARTESIAN_POINT('Ctrl Pts',(271.586966582698,166.787408667143,245.317836348554));
#22161=CARTESIAN_POINT('Ctrl Pts',(271.574982626359,166.777778120583,245.37057049282));
#22162=CARTESIAN_POINT('Ctrl Pts',(271.560043193778,166.76539664204,245.473637636457));
#22163=CARTESIAN_POINT('Ctrl Pts',(271.556438188452,166.762164789129,245.523509871061));
#22164=CARTESIAN_POINT('Ctrl Pts',(271.55643258748,166.762292619895,245.667442907478));
#22165=CARTESIAN_POINT('Ctrl Pts',(271.568995478808,166.773849868396,245.766443228675));
#22166=CARTESIAN_POINT('Ctrl Pts',(271.61558117159,166.809206732078,245.923804651634));
#22167=CARTESIAN_POINT('Ctrl Pts',(271.637087947791,166.824806138798,245.978365805299));
#22168=CARTESIAN_POINT('Ctrl Pts',(271.691169706672,166.86148543902,246.087229534119));
#22169=CARTESIAN_POINT('Ctrl Pts',(271.724610650449,166.882940639207,246.140929653169));
#22170=CARTESIAN_POINT('Ctrl Pts',(271.782739548805,166.91764677583,246.21720597302));
#22171=CARTESIAN_POINT('Ctrl Pts',(271.804221139898,166.930053723957,246.242605470457));
#22172=CARTESIAN_POINT('Ctrl Pts',(271.849038598827,166.954999092752,246.290460601381));
#22173=CARTESIAN_POINT('Ctrl Pts',(271.872566932792,166.967570662237,246.313212577002));
#22174=CARTESIAN_POINT('Ctrl Pts',(271.940175194779,167.001184817018,246.372197845412));
#22175=CARTESIAN_POINT('Ctrl Pts',(271.986560015145,167.021862823293,246.406000105603));
#22176=CARTESIAN_POINT('Ctrl Pts',(272.07297828234,167.05536024451,246.457744032173));
#22177=CARTESIAN_POINT('Ctrl Pts',(272.111589459784,167.06882634101,246.477508148981));
#22178=CARTESIAN_POINT('Ctrl Pts',(272.181627165386,167.09027677835,246.507530839585));
#22179=CARTESIAN_POINT('Ctrl Pts',(272.212340024415,167.098771169116,246.518909668632));
#22180=CARTESIAN_POINT('Ctrl Pts',(272.337848654154,167.129509677067,246.558247879178));
#22181=CARTESIAN_POINT('Ctrl Pts',(272.436921655125,167.145040668581,246.573593133537));
#22182=CARTESIAN_POINT('Ctrl Pts',(272.537988956524,167.150295231825,246.573593133703));
#22183=CARTESIAN_POINT('Origin',(272.715792356506,163.654816037539,244.073593133703));
#22184=CARTESIAN_POINT('Origin',(272.715792356506,163.654816037539,244.073593133703));
#22185=CARTESIAN_POINT('',(272.860336397617,160.81319043826,242.073593133703));
#22186=CARTESIAN_POINT('',(272.918996332834,159.659980853954,244.073593133703));
#22187=CARTESIAN_POINT('Origin',(272.715792356506,163.654816037539,242.073593133703));
#22188=CARTESIAN_POINT('Origin',(272.715792356506,163.654816037539,244.073593133703));
#22189=CARTESIAN_POINT('Origin',(272.715792356506,163.654816037539,275.073593133703));
#22190=CARTESIAN_POINT('',(272.918996332834,159.659980853954,271.473593133703));
#22191=CARTESIAN_POINT('Origin',(272.715792356506,163.654816037539,271.473593133703));
#22192=CARTESIAN_POINT('',(272.918996332834,159.659980853954,275.073593133703));
#22193=CARTESIAN_POINT('Ctrl Pts',(272.918996199032,159.659983271947,247.073589666413));
#22194=CARTESIAN_POINT('Ctrl Pts',(273.153859212278,159.671927547002,247.073336255209));
#22195=CARTESIAN_POINT('Ctrl Pts',(273.372660288957,159.70377047134,247.036490765957));
#22196=CARTESIAN_POINT('Ctrl Pts',(273.673764602282,159.769864517502,246.926335097092));
#22197=CARTESIAN_POINT('Ctrl Pts',(273.769654298301,159.794962976943,246.880468634973));
#22198=CARTESIAN_POINT('Ctrl Pts',(273.952361524276,159.849558183586,246.770439899072));
#22199=CARTESIAN_POINT('Ctrl Pts',(274.037664357212,159.878484631533,246.707630692229));
#22200=CARTESIAN_POINT('Ctrl Pts',(274.28926051078,159.972928496558,246.48357204053));
#22201=CARTESIAN_POINT('Ctrl Pts',(274.410961576191,160.030666872069,246.320599865048));
#22202=CARTESIAN_POINT('Ctrl Pts',(274.571815296306,160.110350675333,245.967456032054));
#22203=CARTESIAN_POINT('Ctrl Pts',(274.611156238513,160.132374288436,245.777012017024));
#22204=CARTESIAN_POINT('Ctrl Pts',(274.611768955062,160.132704049148,245.370016379345));
#22205=CARTESIAN_POINT('Ctrl Pts',(274.572653255307,160.110784343642,245.179908713947));
#22206=CARTESIAN_POINT('Ctrl Pts',(274.451745863215,160.050861447959,244.914832446015));
#22207=CARTESIAN_POINT('Ctrl Pts',(274.401003972674,160.026507080061,244.829821228398));
#22208=CARTESIAN_POINT('Ctrl Pts',(274.308388844366,159.98537773619,244.707325709514));
#22209=CARTESIAN_POINT('Ctrl Pts',(274.274764428741,159.970910463762,244.667330754476));
#22210=CARTESIAN_POINT('Ctrl Pts',(274.201852739805,159.940899138132,244.58901461358));
#22211=CARTESIAN_POINT('Ctrl Pts',(274.161544916096,159.924972533663,244.549787659307));
#22212=CARTESIAN_POINT('Ctrl Pts',(273.791046797412,159.786025320408,244.220670026599));
#22213=CARTESIAN_POINT('Ctrl Pts',(273.387920330164,159.683833457748,244.074128067476));
#22214=CARTESIAN_POINT('Ctrl Pts',(272.918996332834,159.659980853954,244.073593133703));
#22215=CARTESIAN_POINT('Ctrl Pts',(272.512586298077,167.649648688282,247.073589199254));
#22216=CARTESIAN_POINT('Ctrl Pts',(272.277568574454,167.637696415093,247.073269716825));
#22217=CARTESIAN_POINT('Ctrl Pts',(272.058691859226,167.605823019205,247.036390577157));
#22218=CARTESIAN_POINT('Ctrl Pts',(271.757589019498,167.539710588633,246.926232368273));
#22219=CARTESIAN_POINT('Ctrl Pts',(271.661718756569,167.514610376932,246.880373048748));
#22220=CARTESIAN_POINT('Ctrl Pts',(271.524744064579,167.473673830181,246.797874194614));
#22221=CARTESIAN_POINT('Ctrl Pts',(271.480222547247,167.459479498864,246.768089597428));
#22222=CARTESIAN_POINT('Ctrl Pts',(271.393448260767,167.430197197099,246.703950444775));
#22223=CARTESIAN_POINT('Ctrl Pts',(271.352014487236,167.415416685365,246.670325582074));
#22224=CARTESIAN_POINT('Ctrl Pts',(271.142288519241,167.336690915954,246.483479342273));
#22225=CARTESIAN_POINT('Ctrl Pts',(271.020563643374,167.278937434362,246.320448669587));
#22226=CARTESIAN_POINT('Ctrl Pts',(270.859706968011,167.199248759337,245.967279962524));
#22227=CARTESIAN_POINT('Ctrl Pts',(270.820388289757,167.177236159359,245.776985842833));
#22228=CARTESIAN_POINT('Ctrl Pts',(270.819857455755,167.176950467535,245.369914584485));
#22229=CARTESIAN_POINT('Ctrl Pts',(270.858993403178,167.198880150875,245.179793889859));
#22230=CARTESIAN_POINT('Ctrl Pts',(270.979899936523,167.258800041995,244.914735249744));
#22231=CARTESIAN_POINT('Ctrl Pts',(271.03063625638,167.283150543605,244.829736103342));
#22232=CARTESIAN_POINT('Ctrl Pts',(271.123234505968,167.324271049542,244.707267984196));
#22233=CARTESIAN_POINT('Ctrl Pts',(271.156851871753,167.338734878646,244.667283711224));
#22234=CARTESIAN_POINT('Ctrl Pts',(271.22974649002,167.368738646529,244.588992032097));
#22235=CARTESIAN_POINT('Ctrl Pts',(271.270071590961,167.38467151604,244.54975425391));
#22236=CARTESIAN_POINT('Ctrl Pts',(271.640320174432,167.523524687871,244.220906926231));
#22237=CARTESIAN_POINT('Ctrl Pts',(272.043430543987,167.625786722725,244.074366090943));
#22238=CARTESIAN_POINT('Ctrl Pts',(272.512588380178,167.649651221123,244.073593133703));
#22239=CARTESIAN_POINT('Origin',(272.715792356506,163.654816037539,271.473593133703));
#22240=CARTESIAN_POINT('',(272.949476929283,159.060755576417,272.073593133703));
#22241=CARTESIAN_POINT('Origin',(272.715792356506,163.654816037539,272.073593133703));
#22242=CARTESIAN_POINT('Origin',(272.949476929283,159.060755576417,271.473593133703));
#22243=CARTESIAN_POINT('Origin',(272.715792356506,163.654816037539,275.073593133703));
#22244=CARTESIAN_POINT('',(272.360185397933,170.645777608812,274.073593133703));
#22245=CARTESIAN_POINT('',(273.071399315079,156.663854466266,274.073593133703));
#22246=CARTESIAN_POINT('Origin',(272.715792356506,163.654816037539,274.073593133703));
#22247=CARTESIAN_POINT('Origin',(272.715792356506,163.654816037539,274.073593133703));
#22248=CARTESIAN_POINT('',(273.071399315079,156.663854466266,272.073593133703));
#22249=CARTESIAN_POINT('',(273.071399315079,156.663854466266,275.073593133703));
#22250=CARTESIAN_POINT('Origin',(272.715792356506,163.654816037539,272.073593133703));
#22251=CARTESIAN_POINT('Origin',(272.715792356506,163.654816037539,275.073593133703));
#22252=CARTESIAN_POINT('',(272.410986392015,169.647068812916,275.073593133703));
#22253=CARTESIAN_POINT('',(272.410986392015,169.647068812916,275.073593133703));
#22254=CARTESIAN_POINT('Origin',(272.715792356506,163.654816037539,275.073593133703));
#22255=CARTESIAN_POINT('Origin',(272.715792356506,163.654816037539,275.073593133703));
#22256=CARTESIAN_POINT('Origin',(265.724830785233,163.299209078966,272.073593133703));
#22257=CARTESIAN_POINT('Origin',(269.874166757227,163.510271996428,242.073593133703));
#22258=CARTESIAN_POINT('Ctrl Pts',(272.537990127326,167.15027224704,244.573617786368));
#22259=CARTESIAN_POINT('Ctrl Pts',(272.270838725555,167.135913146026,244.57412083749));
#22260=CARTESIAN_POINT('Ctrl Pts',(272.017728127825,167.04749131815,244.68441000503));
#22261=CARTESIAN_POINT('Ctrl Pts',(271.661748083804,166.851990955301,245.049509635926));
#22262=CARTESIAN_POINT('Ctrl Pts',(271.55611035357,166.761907972125,245.307954643826));
#22263=CARTESIAN_POINT('Ctrl Pts',(271.556836124868,166.762470709359,245.840602772399));
#22264=CARTESIAN_POINT('Ctrl Pts',(271.662037569487,166.852212221811,246.097805133848));
#22265=CARTESIAN_POINT('Ctrl Pts',(272.018209844694,167.047687432538,246.463439756173));
#22266=CARTESIAN_POINT('Ctrl Pts',(272.272038834089,167.136250717223,246.573505429044));
#22267=CARTESIAN_POINT('Ctrl Pts',(272.806923706075,167.164444040832,246.573629303778));
#22268=CARTESIAN_POINT('Ctrl Pts',(273.066694910078,167.100701693133,246.462786768509));
#22269=CARTESIAN_POINT('Ctrl Pts',(273.439642900624,166.942402854417,246.097308333644));
#22270=CARTESIAN_POINT('Ctrl Pts',(273.554253080628,166.863527017937,245.838716869155));
#22271=CARTESIAN_POINT('Ctrl Pts',(273.553385901434,166.864049105555,245.306031962191));
#22272=CARTESIAN_POINT('Ctrl Pts',(273.439055352264,166.942671346622,245.049123050581));
#22273=CARTESIAN_POINT('Ctrl Pts',(273.06614841851,167.100905306649,244.684044657033));
#22274=CARTESIAN_POINT('Ctrl Pts',(272.805141529096,167.164631348054,244.573114735247));
#22275=CARTESIAN_POINT('Ctrl Pts',(272.537990127326,167.15027224704,244.573617786368));
#22276=CARTESIAN_POINT('Ctrl Pts',(272.512392795351,167.653496269653,244.069743136217));
#22277=CARTESIAN_POINT('Ctrl Pts',(272.052943198304,167.629244750519,244.070499666465));
#22278=CARTESIAN_POINT('Ctrl Pts',(271.615392455326,167.52056496946,244.236362023006));
#22279=CARTESIAN_POINT('Ctrl Pts',(270.99797829939,167.28622785556,244.785430835153));
#22280=CARTESIAN_POINT('Ctrl Pts',(270.813822756294,167.179955747015,245.17410776262));
#22281=CARTESIAN_POINT('Ctrl Pts',(270.815086319005,167.180621532238,245.975140557769));
#22282=CARTESIAN_POINT('Ctrl Pts',(270.998482266767,167.286489787197,246.361948740322));
#22283=CARTESIAN_POINT('Ctrl Pts',(271.616225886466,167.520803660008,246.911822009124));
#22284=CARTESIAN_POINT('Ctrl Pts',(272.055013894835,167.629666405863,247.07734829438));
#22285=CARTESIAN_POINT('Ctrl Pts',(272.974900726542,167.677585388617,247.077534615452));
#22286=CARTESIAN_POINT('Ctrl Pts',(273.419449544341,167.6121630998,246.91084003692));
#22287=CARTESIAN_POINT('Ctrl Pts',(274.055683582988,167.441736047101,246.361201561415));
#22288=CARTESIAN_POINT('Ctrl Pts',(274.25032046597,167.354736271579,245.972304495464));
#22289=CARTESIAN_POINT('Ctrl Pts',(274.24884561165,167.35530895384,245.171216143361));
#22290=CARTESIAN_POINT('Ctrl Pts',(274.054681825528,167.442026420456,244.784849461951));
#22291=CARTESIAN_POINT('Ctrl Pts',(273.418516406651,167.612380366725,244.235812573376));
#22292=CARTESIAN_POINT('Ctrl Pts',(272.971842392397,167.677747788788,244.06898660597));
#22293=CARTESIAN_POINT('Ctrl Pts',(272.512392795351,167.653496269653,244.069743136217));
#22294=CARTESIAN_POINT('Ctrl Pts',(272.893594585687,160.159359828037,244.573617786368));
#22295=CARTESIAN_POINT('Ctrl Pts',(273.160745987457,160.173718929051,244.57412083749));
#22296=CARTESIAN_POINT('Ctrl Pts',(273.413856585187,160.262140756928,244.68441000503));
#22297=CARTESIAN_POINT('Ctrl Pts',(273.769836629208,160.457641119777,245.049509635926));
#22298=CARTESIAN_POINT('Ctrl Pts',(273.875474359442,160.547724102953,245.307954643826));
#22299=CARTESIAN_POINT('Ctrl Pts',(273.874748588144,160.547161365719,245.840602772399));
#22300=CARTESIAN_POINT('Ctrl Pts',(273.769547143525,160.457419853267,246.097805133848));
#22301=CARTESIAN_POINT('Ctrl Pts',(273.413374868318,160.26194464254,246.463439756173));
#22302=CARTESIAN_POINT('Ctrl Pts',(273.159545878923,160.173381357855,246.573505429044));
#22303=CARTESIAN_POINT('Ctrl Pts',(272.624661006937,160.145188034246,246.573629303778));
#22304=CARTESIAN_POINT('Ctrl Pts',(272.364889802934,160.208930381945,246.462786768509));
#22305=CARTESIAN_POINT('Ctrl Pts',(271.991941812388,160.367229220661,246.097308333644));
#22306=CARTESIAN_POINT('Ctrl Pts',(271.877331632384,160.446105057141,245.838716869155));
#22307=CARTESIAN_POINT('Ctrl Pts',(271.878198811578,160.445582969523,245.306031962191));
#22308=CARTESIAN_POINT('Ctrl Pts',(271.992529360748,160.366960728456,245.049123050581));
#22309=CARTESIAN_POINT('Ctrl Pts',(272.365436294502,160.208726768429,244.684044657033));
#22310=CARTESIAN_POINT('Ctrl Pts',(272.626443183916,160.145000727024,244.573114735247));
#22311=CARTESIAN_POINT('Ctrl Pts',(272.893594585687,160.159359828037,244.573617786368));
#22312=CARTESIAN_POINT('Ctrl Pts',(272.919202378768,159.655930148048,244.069537212942));
#22313=CARTESIAN_POINT('Ctrl Pts',(273.378730564158,159.680185710011,244.070293846782));
#22314=CARTESIAN_POINT('Ctrl Pts',(273.816356684055,159.788873770082,244.236178914949));
#22315=CARTESIAN_POINT('Ctrl Pts',(274.433877682772,160.023226755769,244.785322911543));
#22316=CARTESIAN_POINT('Ctrl Pts',(274.618065314493,160.129505480478,245.174053062134));
#22317=CARTESIAN_POINT('Ctrl Pts',(274.616801531998,160.128839653142,245.975195540614));
#22318=CARTESIAN_POINT('Ctrl Pts',(274.433373627741,160.022964807513,246.362056690417));
#22319=CARTESIAN_POINT('Ctrl Pts',(273.815523109177,159.788635062134,246.91200525379));
#22320=CARTESIAN_POINT('Ctrl Pts',(273.376659511836,159.679764020304,247.077554204665));
#22321=CARTESIAN_POINT('Ctrl Pts',(272.456615337694,159.631836976076,247.077740551258));
#22322=CARTESIAN_POINT('Ctrl Pts',(272.011991005059,159.697259951451,246.911023147137));
#22323=CARTESIAN_POINT('Ctrl Pts',(271.375649366784,159.867691960703,246.361309409185));
#22324=CARTESIAN_POINT('Ctrl Pts',(271.180979778523,159.954695056313,245.972359089997));
#22325=CARTESIAN_POINT('Ctrl Pts',(271.182454881187,159.954122353375,245.17116104689));
#22326=CARTESIAN_POINT('Ctrl Pts',(271.376651293522,159.867401578405,244.784741458735));
#22327=CARTESIAN_POINT('Ctrl Pts',(272.012924300764,159.697042678946,244.235629390082));
#22328=CARTESIAN_POINT('Ctrl Pts',(272.459674193378,159.631674586084,244.068780579103));
#22329=CARTESIAN_POINT('Ctrl Pts',(272.919202378768,159.655930148048,244.069537212942));
#22330=CARTESIAN_POINT('',(0.,0.,0.));
#22331=CARTESIAN_POINT('Origin',(272.351065622502,161.693151647739,245.488927842219));
#22332=CARTESIAN_POINT('',(269.715877188101,158.727024455329,244.98111745079));
#22333=CARTESIAN_POINT('Origin',(269.057080079501,157.985492657226,244.854164852932));
#22334=CARTESIAN_POINT('',(269.42850336885,164.376574551399,244.98111745079));
#22335=CARTESIAN_POINT('Origin',(272.351065622502,161.693151647739,245.488927842219));
#22336=CARTESIAN_POINT('Origin',(268.697862805437,165.047430277314,244.854164852932));
#22337=CARTESIAN_POINT('Origin',(267.097176680551,177.288521295714,244.675902705153));
#22338=CARTESIAN_POINT('',(264.46198824615,174.322394103304,244.168092313724));
#22339=CARTESIAN_POINT('Origin',(263.80319113755,173.580862305201,244.041139715866));
#22340=CARTESIAN_POINT('',(271.027099880217,177.48842341536,245.394055047827));
#22341=CARTESIAN_POINT('Origin',(267.097176680551,177.288521295714,244.675902705153));
#22342=CARTESIAN_POINT('Origin',(272.009580680134,177.538398945271,245.573593133495));
#22343=CARTESIAN_POINT('Origin',(269.931407552539,154.489861883276,244.98111745079));
#22344=CARTESIAN_POINT('',(270.662048115952,153.819006157361,245.108070048647));
#22345=CARTESIAN_POINT('',(269.742185248056,154.489861883276,245.963051725314));
#22346=CARTESIAN_POINT('Origin',(269.931407552539,154.489861883276,244.98111745079));
#22347=CARTESIAN_POINT('Origin',(269.931407552539,154.489861883276,244.98111745079));
#22348=CARTESIAN_POINT('',(269.931407552539,154.489861883276,243.98111745079));
#22349=CARTESIAN_POINT('Origin',(269.931407552539,154.489861883276,244.98111745079));
#22350=CARTESIAN_POINT('Origin',(273.381207520346,150.573261456076,245.573593133495));
#22351=CARTESIAN_POINT('',(272.398726720429,150.523285926165,245.394055047827));
#22352=CARTESIAN_POINT('',(274.379916316242,150.624062450158,245.573593133495));
#22353=CARTESIAN_POINT('Origin',(273.381207520346,150.573261456076,245.573593133495));
#22354=CARTESIAN_POINT('Origin',(273.381207520346,150.573261456076,245.573593133495));
#22355=CARTESIAN_POINT('',(274.381207520346,150.573261456076,245.573593133495));
#22356=CARTESIAN_POINT('Origin',(273.381207520346,150.573261456076,245.573593133495));
#22357=CARTESIAN_POINT('Origin',(270.590204661139,155.231393681379,245.108070048647));
#22358=CARTESIAN_POINT('',(271.320845224552,154.560537955464,245.235022646504));
#22359=CARTESIAN_POINT('',(271.320845224552,154.560537955464,245.235022646504));
#22360=CARTESIAN_POINT('',(269.859564097726,155.902249407294,244.98111745079));
#22361=CARTESIAN_POINT('Origin',(270.590204661139,155.231393681379,245.108070048647));
#22362=CARTESIAN_POINT('Origin',(270.590204661139,155.231393681379,245.108070048647));
#22363=CARTESIAN_POINT('Origin',(269.057080079501,157.985492657226,244.854164852932));
#22364=CARTESIAN_POINT('',(271.177158314927,157.385313003499,245.235022646504));
#22365=CARTESIAN_POINT('Origin',(270.518361206326,156.643781205396,245.108070048647));
#22366=CARTESIAN_POINT('',(269.715877188101,158.727024455329,244.98111745079));
#22367=CARTESIAN_POINT('Origin',(270.518361206326,156.643781205396,245.108070048647));
#22368=CARTESIAN_POINT('Origin',(270.015457022638,166.530493873519,245.108070048647));
#22369=CARTESIAN_POINT('',(270.74609758605,165.859638147604,245.235022646504));
#22370=CARTESIAN_POINT('',(270.74609758605,165.859638147604,245.235022646504));
#22371=CARTESIAN_POINT('',(269.284816459225,167.201349599434,244.98111745079));
#22372=CARTESIAN_POINT('Origin',(270.015457022638,166.530493873519,245.108070048647));
#22373=CARTESIAN_POINT('Origin',(270.015457022638,166.530493873519,245.108070048647));
#22374=CARTESIAN_POINT('Origin',(263.80319113755,173.580862305201,244.041139715866));
#22375=CARTESIAN_POINT('',(270.602410676425,168.68441319564,245.235022646504));
#22376=CARTESIAN_POINT('Origin',(269.943613567825,167.942881397537,245.108070048647));
#22377=CARTESIAN_POINT('',(264.46198824615,174.322394103304,244.168092313724));
#22378=CARTESIAN_POINT('Origin',(269.943613567825,167.942881397537,245.108070048647));
#22379=CARTESIAN_POINT('Origin',(273.432008514428,149.57455266018,245.573593133495));
#22380=CARTESIAN_POINT('',(272.449527714511,149.524577130268,245.394055047827));
#22381=CARTESIAN_POINT('Ctrl Pts',(269.859564097726,155.902249407293,244.98111745079));
#22382=CARTESIAN_POINT('Ctrl Pts',(269.859564097726,155.902249407293,244.98111745079));
#22383=CARTESIAN_POINT('Ctrl Pts',(269.859564097726,155.902249407294,244.98111745079));
#22384=CARTESIAN_POINT('Ctrl Pts',(269.680257832371,155.893128694066,245.964868474065));
#22385=CARTESIAN_POINT('Ctrl Pts',(269.680257832371,155.893128694066,245.964868474065));
#22386=CARTESIAN_POINT('Ctrl Pts',(269.680257832371,155.893128694066,245.964868474065));
#22387=CARTESIAN_POINT('Ctrl Pts',(270.339054940971,156.634660492169,246.091821071922));
#22388=CARTESIAN_POINT('Ctrl Pts',(271.069695504384,155.963804766254,246.218773669779));
#22389=CARTESIAN_POINT('Ctrl Pts',(270.410898395784,155.222272968151,246.091821071922));
#22390=CARTESIAN_POINT('Ctrl Pts',(270.997852049571,157.376192290271,246.218773669779));
#22391=CARTESIAN_POINT('Ctrl Pts',(272.459133176397,156.034480838441,246.472678865494));
#22392=CARTESIAN_POINT('Ctrl Pts',(271.141538959196,154.551417242236,246.218773669779));
#22393=CARTESIAN_POINT('Ctrl Pts',(271.177158314927,157.385313003499,245.235022646504));
#22394=CARTESIAN_POINT('Ctrl Pts',(272.638439441753,156.043601551669,245.488927842219));
#22395=CARTESIAN_POINT('Ctrl Pts',(271.320845224552,154.560537955463,245.235022646504));
#22396=CARTESIAN_POINT('Ctrl Pts',(271.356464580282,157.394433716726,244.251271623229));
#22397=CARTESIAN_POINT('Ctrl Pts',(272.817745707108,156.052722264896,244.505176818944));
#22398=CARTESIAN_POINT('Ctrl Pts',(271.500151489907,154.569658668691,244.251271623229));
#22399=CARTESIAN_POINT('Ctrl Pts',(270.697667471682,156.652901918624,244.124319025372));
#22400=CARTESIAN_POINT('Ctrl Pts',(271.428308035095,155.982046192709,244.251271623229));
#22401=CARTESIAN_POINT('Ctrl Pts',(270.769510926494,155.240514394606,244.124319025372));
#22402=CARTESIAN_POINT('Ctrl Pts',(270.038870363082,155.911370120521,243.997366427515));
#22403=CARTESIAN_POINT('Ctrl Pts',(270.038870363082,155.911370120521,243.997366427515));
#22404=CARTESIAN_POINT('Ctrl Pts',(270.038870363082,155.911370120521,243.997366427515));
#22405=CARTESIAN_POINT('Ctrl Pts',(269.859564097726,155.902249407293,244.98111745079));
#22406=CARTESIAN_POINT('Ctrl Pts',(269.859564097726,155.902249407293,244.98111745079));
#22407=CARTESIAN_POINT('Ctrl Pts',(269.859564097726,155.902249407294,244.98111745079));
#22408=CARTESIAN_POINT('Ctrl Pts',(269.284816459225,167.201349599434,244.98111745079));
#22409=CARTESIAN_POINT('Ctrl Pts',(269.284816459225,167.201349599434,244.98111745079));
#22410=CARTESIAN_POINT('Ctrl Pts',(269.284816459225,167.201349599434,244.98111745079));
#22411=CARTESIAN_POINT('Ctrl Pts',(269.105510193869,167.192228886207,245.964868474065));
#22412=CARTESIAN_POINT('Ctrl Pts',(269.105510193869,167.192228886207,245.964868474065));
#22413=CARTESIAN_POINT('Ctrl Pts',(269.105510193869,167.192228886207,245.964868474065));
#22414=CARTESIAN_POINT('Ctrl Pts',(269.764307302469,167.93376068431,246.091821071922));
#22415=CARTESIAN_POINT('Ctrl Pts',(270.494947865883,167.262904958394,246.218773669779));
#22416=CARTESIAN_POINT('Ctrl Pts',(269.836150757282,166.521373160292,246.091821071922));
#22417=CARTESIAN_POINT('Ctrl Pts',(270.423104411069,168.675292482413,246.218773669779));
#22418=CARTESIAN_POINT('Ctrl Pts',(271.884385537896,167.333581030582,246.472678865494));
#22419=CARTESIAN_POINT('Ctrl Pts',(270.566791320695,165.850517434376,246.218773669779));
#22420=CARTESIAN_POINT('Ctrl Pts',(270.602410676424,168.68441319564,245.235022646504));
#22421=CARTESIAN_POINT('Ctrl Pts',(272.063691803252,167.34270174381,245.488927842219));
#22422=CARTESIAN_POINT('Ctrl Pts',(270.74609758605,165.859638147604,245.235022646504));
#22423=CARTESIAN_POINT('Ctrl Pts',(270.78171694178,168.693533908868,244.251271623229));
#22424=CARTESIAN_POINT('Ctrl Pts',(272.242998068607,167.351822457037,244.505176818944));
#22425=CARTESIAN_POINT('Ctrl Pts',(270.925403851406,165.868758860831,244.251271623229));
#22426=CARTESIAN_POINT('Ctrl Pts',(270.12291983318,167.952002110765,244.124319025372));
#22427=CARTESIAN_POINT('Ctrl Pts',(270.853560396594,167.28114638485,244.25127162323));
#22428=CARTESIAN_POINT('Ctrl Pts',(270.194763287993,166.539614586747,244.124319025372));
#22429=CARTESIAN_POINT('Ctrl Pts',(269.46412272458,167.210470312662,243.997366427515));
#22430=CARTESIAN_POINT('Ctrl Pts',(269.46412272458,167.210470312662,243.997366427515));
#22431=CARTESIAN_POINT('Ctrl Pts',(269.46412272458,167.210470312662,243.997366427515));
#22432=CARTESIAN_POINT('Ctrl Pts',(269.284816459225,167.201349599434,244.98111745079));
#22433=CARTESIAN_POINT('Ctrl Pts',(269.284816459225,167.201349599434,244.98111745079));
#22434=CARTESIAN_POINT('Ctrl Pts',(269.284816459225,167.201349599434,244.98111745079));
#22435=CARTESIAN_POINT('Origin',(238.067118190679,151.504231246999,245.983333506556));
#22436=CARTESIAN_POINT('',(241.032274232146,152.585076330075,248.440898064434));
#22437=CARTESIAN_POINT('Origin',(241.773563242513,152.855287600844,249.055289203903));
#22438=CARTESIAN_POINT('',(237.128624750255,148.490992705803,248.440898064434));
#22439=CARTESIAN_POINT('Origin',(238.067118190679,151.504231246999,245.983333506556));
#22440=CARTESIAN_POINT('Origin',(236.894001390149,147.737683070505,249.055289203903));
#22441=CARTESIAN_POINT('Origin',(228.757252972023,138.49174626232,249.917994543901));
#22442=CARTESIAN_POINT('',(231.722409013491,139.572591345396,252.375559101779));
#22443=CARTESIAN_POINT('Origin',(232.463698023858,139.842802616165,252.989950241249));
#22444=CARTESIAN_POINT('',(227.324186103648,139.858154780476,246.442473415743));
#22445=CARTESIAN_POINT('Origin',(228.757252972023,138.49174626232,249.917994543901));
#22446=CARTESIAN_POINT('Origin',(226.965919386554,140.199756910015,245.573593133703));
#22447=CARTESIAN_POINT('Origin',(243.960011343564,155.655639048279,248.440898064434));
#22448=CARTESIAN_POINT('',(244.19463470367,156.408948683578,247.826506924964));
#22449=CARTESIAN_POINT('',(243.321882482923,155.655639048279,249.210827643822));
#22450=CARTESIAN_POINT('Origin',(243.960011343564,155.655639048279,248.440898064434));
#22451=CARTESIAN_POINT('Origin',(243.960011343564,155.655639048279,248.440898064434));
#22452=CARTESIAN_POINT('',(243.960011343564,155.655639048279,249.440898064434));
#22453=CARTESIAN_POINT('Origin',(243.960011343564,155.655639048279,248.440898064434));
#22454=CARTESIAN_POINT('Origin',(245.597924271693,159.74069839092,245.573593133703));
#22455=CARTESIAN_POINT('',(244.874185698326,160.430772645925,245.573593133703));
#22456=CARTESIAN_POINT('',(245.956190988787,159.399096261381,246.442473415743));
#22457=CARTESIAN_POINT('Origin',(245.597924271693,159.74069839092,245.573593133703));
#22458=CARTESIAN_POINT('',(246.597924271693,159.74069839092,245.573593133703));
#22459=CARTESIAN_POINT('Origin',(245.597924271693,159.74069839092,245.573593133703));
#22460=CARTESIAN_POINT('Origin',(245.597924271693,159.74069839092,245.573593133703));
#22461=CARTESIAN_POINT('Origin',(243.218722333198,155.38542777751,247.826506924964));
#22462=CARTESIAN_POINT('',(243.453345693303,156.138737412809,247.212115785495));
#22463=CARTESIAN_POINT('',(243.453345693303,156.138737412809,247.212115785495));
#22464=CARTESIAN_POINT('',(242.984098973092,154.632118142211,248.440898064434));
#22465=CARTESIAN_POINT('Origin',(243.218722333198,155.38542777751,247.826506924964));
#22466=CARTESIAN_POINT('Origin',(243.218722333198,155.38542777751,247.826506924964));
#22467=CARTESIAN_POINT('Origin',(241.773563242513,152.855287600844,249.055289203903));
#22468=CARTESIAN_POINT('',(241.501520952358,154.091695600673,247.212115785495));
#22469=CARTESIAN_POINT('Origin',(242.242809962725,154.361906871442,247.826506924964));
#22470=CARTESIAN_POINT('',(241.032274232146,152.585076330075,248.440898064434));
#22471=CARTESIAN_POINT('Origin',(242.242809962725,154.361906871442,247.826506924964));
#22472=CARTESIAN_POINT('Origin',(235.411423369415,147.197260528966,247.826506924964));
#22473=CARTESIAN_POINT('',(235.646046729521,147.950570164265,247.212115785495));
#22474=CARTESIAN_POINT('',(235.646046729521,147.950570164265,247.212115785495));
#22475=CARTESIAN_POINT('',(235.176800009309,146.443950893667,248.440898064434));
#22476=CARTESIAN_POINT('Origin',(235.411423369415,147.197260528966,247.826506924964));
#22477=CARTESIAN_POINT('Origin',(235.411423369415,147.197260528966,247.826506924964));
#22478=CARTESIAN_POINT('Origin',(232.463698023858,139.842802616165,252.989950241249));
#22479=CARTESIAN_POINT('',(233.694221988576,145.903528352129,247.212115785495));
#22480=CARTESIAN_POINT('Origin',(234.435510998943,146.173739622898,247.826506924964));
#22481=CARTESIAN_POINT('',(231.722409013491,139.572591345396,252.375559101779));
#22482=CARTESIAN_POINT('Origin',(234.435510998943,146.173739622898,247.826506924964));
#22483=CARTESIAN_POINT('Origin',(246.287998526698,160.464436964287,245.573593133703));
#22484=CARTESIAN_POINT('',(246.646265243792,160.122834834748,246.442473415743));
#22485=CARTESIAN_POINT('Ctrl Pts',(242.984098973092,154.632118142211,248.440898064434));
#22486=CARTESIAN_POINT('Ctrl Pts',(242.984098973092,154.632118142211,248.440898064434));
#22487=CARTESIAN_POINT('Ctrl Pts',(242.984098973092,154.632118142211,248.440898064434));
#22488=CARTESIAN_POINT('Ctrl Pts',(242.355256797342,155.231710055528,248.935920342198));
#22489=CARTESIAN_POINT('Ctrl Pts',(242.355256797342,155.231710055528,248.935920342198));
#22490=CARTESIAN_POINT('Ctrl Pts',(242.355256797342,155.231710055528,248.935920342198));
#22491=CARTESIAN_POINT('Ctrl Pts',(241.613967786975,154.961498784759,248.321529202729));
#22492=CARTESIAN_POINT('Ctrl Pts',(241.848591147081,155.714808420058,247.707138063259));
#22493=CARTESIAN_POINT('Ctrl Pts',(242.589880157448,155.985019690827,248.321529202729));
#22494=CARTESIAN_POINT('Ctrl Pts',(240.872678776608,154.69128751399,247.707138063259));
#22495=CARTESIAN_POINT('Ctrl Pts',(241.34192549682,156.197906784588,246.47835578432));
#22496=CARTESIAN_POINT('Ctrl Pts',(242.824503517554,156.738329326126,247.707138063259));
#22497=CARTESIAN_POINT('Ctrl Pts',(241.501520952358,154.091695600673,247.212115785495));
#22498=CARTESIAN_POINT('Ctrl Pts',(241.97076767257,155.598314871271,245.983333506556));
#22499=CARTESIAN_POINT('Ctrl Pts',(243.453345693303,156.138737412809,247.212115785495));
#22500=CARTESIAN_POINT('Ctrl Pts',(242.130363128108,153.492103687356,246.717093507731));
#22501=CARTESIAN_POINT('Ctrl Pts',(242.59960984832,154.998722957953,245.488311228792));
#22502=CARTESIAN_POINT('Ctrl Pts',(244.082187869053,155.539145499492,246.717093507731));
#22503=CARTESIAN_POINT('Ctrl Pts',(242.871652138475,153.762314958125,247.3314846472));
#22504=CARTESIAN_POINT('Ctrl Pts',(243.106275498581,154.515624593424,246.717093507731));
#22505=CARTESIAN_POINT('Ctrl Pts',(243.847564508947,154.785835864193,247.3314846472));
#22506=CARTESIAN_POINT('Ctrl Pts',(243.612941148842,154.032526228894,247.94587578667));
#22507=CARTESIAN_POINT('Ctrl Pts',(243.612941148842,154.032526228894,247.94587578667));
#22508=CARTESIAN_POINT('Ctrl Pts',(243.612941148842,154.032526228894,247.94587578667));
#22509=CARTESIAN_POINT('Ctrl Pts',(242.984098973092,154.632118142211,248.440898064434));
#22510=CARTESIAN_POINT('Ctrl Pts',(242.984098973092,154.632118142211,248.440898064434));
#22511=CARTESIAN_POINT('Ctrl Pts',(242.984098973092,154.632118142211,248.440898064434));
#22512=CARTESIAN_POINT('Ctrl Pts',(235.176800009309,146.443950893667,248.440898064434));
#22513=CARTESIAN_POINT('Ctrl Pts',(235.176800009309,146.443950893667,248.440898064434));
#22514=CARTESIAN_POINT('Ctrl Pts',(235.176800009309,146.443950893667,248.440898064434));
#22515=CARTESIAN_POINT('Ctrl Pts',(234.547957833559,147.043542806985,248.935920342198));
#22516=CARTESIAN_POINT('Ctrl Pts',(234.547957833559,147.043542806985,248.935920342198));
#22517=CARTESIAN_POINT('Ctrl Pts',(234.547957833559,147.043542806985,248.935920342198));
#22518=CARTESIAN_POINT('Ctrl Pts',(233.806668823193,146.773331536215,248.321529202729));
#22519=CARTESIAN_POINT('Ctrl Pts',(234.041292183298,147.526641171514,247.707138063259));
#22520=CARTESIAN_POINT('Ctrl Pts',(234.782581193665,147.796852442283,248.321529202729));
#22521=CARTESIAN_POINT('Ctrl Pts',(233.065379812826,146.503120265446,247.707138063259));
#22522=CARTESIAN_POINT('Ctrl Pts',(233.534626533037,148.009739536044,246.47835578432));
#22523=CARTESIAN_POINT('Ctrl Pts',(235.017204553771,148.550162077582,247.707138063259));
#22524=CARTESIAN_POINT('Ctrl Pts',(233.694221988576,145.903528352129,247.212115785495));
#22525=CARTESIAN_POINT('Ctrl Pts',(234.163468708787,147.410147622727,245.983333506556));
#22526=CARTESIAN_POINT('Ctrl Pts',(235.646046729521,147.950570164265,247.212115785495));
#22527=CARTESIAN_POINT('Ctrl Pts',(234.323064164326,145.303936438812,246.717093507731));
#22528=CARTESIAN_POINT('Ctrl Pts',(234.792310884537,146.81055570941,245.488311228792));
#22529=CARTESIAN_POINT('Ctrl Pts',(236.274888905271,147.350978250948,246.717093507731));
#22530=CARTESIAN_POINT('Ctrl Pts',(235.064353174692,145.574147709581,247.3314846472));
#22531=CARTESIAN_POINT('Ctrl Pts',(235.298976534798,146.32745734488,246.717093507731));
#22532=CARTESIAN_POINT('Ctrl Pts',(236.040265545165,146.597668615649,247.3314846472));
#22533=CARTESIAN_POINT('Ctrl Pts',(235.805642185059,145.84435898035,247.94587578667));
#22534=CARTESIAN_POINT('Ctrl Pts',(235.805642185059,145.84435898035,247.94587578667));
#22535=CARTESIAN_POINT('Ctrl Pts',(235.805642185059,145.84435898035,247.94587578667));
#22536=CARTESIAN_POINT('Ctrl Pts',(235.176800009309,146.443950893667,248.440898064434));
#22537=CARTESIAN_POINT('Ctrl Pts',(235.176800009309,146.443950893667,248.440898064434));
#22538=CARTESIAN_POINT('Ctrl Pts',(235.176800009309,146.443950893667,248.440898064434));
#22539=CARTESIAN_POINT('',(0.,0.,0.));
#22540=CARTESIAN_POINT('',(0.,0.,0.));
#22541=CARTESIAN_POINT('',(0.,0.,0.));
#22542=CARTESIAN_POINT('',(0.,0.,0.));
#22543=CARTESIAN_POINT('',(0.,0.,0.));
#22544=CARTESIAN_POINT('',(0.,0.,0.));
#22545=CARTESIAN_POINT('',(0.,0.,0.));
#22546=CARTESIAN_POINT('',(0.,0.,0.));
#22547=CARTESIAN_POINT('',(0.,0.,0.));
#22548=CARTESIAN_POINT('Origin',(239.288983046696,153.123984191663,272.073593133703));
#22549=CARTESIAN_POINT('',(235.453039626143,150.771211768687,272.073593133703));
#22550=CARTESIAN_POINT('Origin',(239.288983046696,153.123984191663,272.073593133703));
#22551=CARTESIAN_POINT('',(235.453039626143,150.771211768687,270.073593133703));
#22552=CARTESIAN_POINT('',(235.453039626143,150.771211768687,272.073593133703));
#22553=CARTESIAN_POINT('Origin',(239.288983046696,153.123984191663,270.073593133703));
#22554=CARTESIAN_POINT('Origin',(272.715792356497,163.654816037544,272.073593133703));
#22555=CARTESIAN_POINT('',(268.453633000327,161.04062445646,272.073593133703));
#22556=CARTESIAN_POINT('Origin',(272.715792356497,163.654816037544,272.073593133703));
#22557=CARTESIAN_POINT('',(268.453633000327,161.04062445646,270.073593133703));
#22558=CARTESIAN_POINT('',(268.453633000327,161.04062445646,272.073593133703));
#22559=CARTESIAN_POINT('Origin',(272.715792356497,163.654816037544,270.073593133703));
#22560=CARTESIAN_POINT('Origin',(239.288983046696,153.123984191663,248.073593133703));
#22561=CARTESIAN_POINT('',(243.12492646725,155.476756614638,248.073593133703));
#22562=CARTESIAN_POINT('Origin',(239.288983046696,153.123984191663,248.073593133703));
#22563=CARTESIAN_POINT('',(243.12492646725,155.476756614638,250.073593133703));
#22564=CARTESIAN_POINT('',(243.12492646725,155.476756614638,248.073593133703));
#22565=CARTESIAN_POINT('Origin',(239.288983046696,153.123984191663,250.073593133703));
#22566=CARTESIAN_POINT('Origin',(272.715792356497,163.654816037544,248.073593133703));
#22567=CARTESIAN_POINT('',(276.977951712667,166.269007618627,248.073593133703));
#22568=CARTESIAN_POINT('Origin',(272.715792356497,163.654816037544,248.073593133703));
#22569=CARTESIAN_POINT('',(276.977951712667,166.269007618627,250.073593133703));
#22570=CARTESIAN_POINT('',(276.977951712667,166.269007618627,248.073593133703));
#22571=CARTESIAN_POINT('Origin',(272.715792356497,163.654816037544,250.073593133703));
#22572=CARTESIAN_POINT('Origin',(297.208732752758,202.139824427113,260.073593133703));
#22573=CARTESIAN_POINT('',(302.437115914926,193.615505714772,260.073593133703));
#22574=CARTESIAN_POINT('Origin',(297.208732752758,202.139824427113,260.073593133703));
#22575=CARTESIAN_POINT('',(280.27388726284,180.021709493136,260.073593133703));
#22576=CARTESIAN_POINT('',(302.437115914926,193.615505714772,260.073593133703));
#22577=CARTESIAN_POINT('',(275.045504100673,188.546028205476,270.073593133703));
#22578=CARTESIAN_POINT('Origin',(275.045504100673,188.546028205476,260.073593133703));
#22579=CARTESIAN_POINT('',(239.243365508842,166.586818924372,270.073593133703));
#22580=CARTESIAN_POINT('',(297.208732752758,202.139824427113,270.073593133703));
#22581=CARTESIAN_POINT('',(236.629173927758,170.848978280542,268.733847171548));
#22582=CARTESIAN_POINT('Origin',(239.243365508842,166.586818924372,260.073593133703));
#22583=CARTESIAN_POINT('',(253.677811352439,181.305744604878,268.733847171548));
#22584=CARTESIAN_POINT('',(236.629173927758,170.848978280542,268.733847171548));
#22585=CARTESIAN_POINT('',(253.677811352439,181.305744604878,251.413339095859));
#22586=CARTESIAN_POINT('Origin',(256.292002933523,177.043585248707,260.073593133703));
#22587=CARTESIAN_POINT('',(236.629173927758,170.848978280542,251.413339095859));
#22588=CARTESIAN_POINT('',(236.629173927758,170.848978280542,251.413339095859));
#22589=CARTESIAN_POINT('',(239.243365508842,166.586818924372,250.073593133703));
#22590=CARTESIAN_POINT('Origin',(239.243365508842,166.586818924372,260.073593133703));
#22591=CARTESIAN_POINT('',(275.045504100673,188.546028205476,250.073593133703));
#22592=CARTESIAN_POINT('',(297.208732752758,202.139824427113,250.073593133703));
#22593=CARTESIAN_POINT('Origin',(275.045504100673,188.546028205476,260.073593133703));
#22594=CARTESIAN_POINT('Origin',(297.208732752758,202.139824427113,260.073593133703));
#22595=CARTESIAN_POINT('',(255.323361884785,182.448125072191,249.2175955373));
#22596=CARTESIAN_POINT('',(255.323361884814,182.448125072217,270.929590730103));
#22597=CARTESIAN_POINT('Origin',(257.996866675991,178.089261881141,260.073593133703));
#22598=CARTESIAN_POINT('',(255.058804871611,182.152775729166,270.982305248339));
#22599=CARTESIAN_POINT('Ctrl Pts',(255.323361885007,182.448125072171,270.929590730169));
#22600=CARTESIAN_POINT('Ctrl Pts',(255.309569700968,182.408536079969,270.942089768565));
#22601=CARTESIAN_POINT('Ctrl Pts',(255.289379287412,182.371026850316,270.952064384874));
#22602=CARTESIAN_POINT('Ctrl Pts',(255.26450099475,182.336243715935,270.959783119772));
#22603=CARTESIAN_POINT('Ctrl Pts',(255.250346319745,182.316453613395,270.964174746858));
#22604=CARTESIAN_POINT('Ctrl Pts',(255.234674366869,182.297545581916,270.967835176688));
#22605=CARTESIAN_POINT('Ctrl Pts',(255.217801828123,182.279635918025,270.970807219426));
#22606=CARTESIAN_POINT('Ctrl Pts',(255.183565204112,182.243294829227,270.976837889219));
#22607=CARTESIAN_POINT('Ctrl Pts',(255.145217910695,182.21112323878,270.980215787129));
#22608=CARTESIAN_POINT('Ctrl Pts',(255.104099246087,182.182404890805,270.981583115665));
#22609=CARTESIAN_POINT('Ctrl Pts',(255.089337425425,182.17209485018,270.982073993928));
#22610=CARTESIAN_POINT('Ctrl Pts',(255.07421853595,182.16222968627,270.982305248323));
#22611=CARTESIAN_POINT('Ctrl Pts',(255.058804871611,182.152775729166,270.982305248339));
#22612=CARTESIAN_POINT('',(236.629173927758,170.848978280542,270.982305248339));
#22613=CARTESIAN_POINT('',(236.629173927758,170.848978280542,270.982305248339));
#22614=CARTESIAN_POINT('',(239.243365508842,166.586818924372,272.073593133703));
#22615=CARTESIAN_POINT('Origin',(239.243365508842,166.586818924372,260.073593133703));
#22616=CARTESIAN_POINT('',(275.045504100673,188.546028205476,272.073593133703));
#22617=CARTESIAN_POINT('',(297.208732752758,202.139824427113,272.073593133703));
#22618=CARTESIAN_POINT('',(278.513621142497,182.891634853029,270.073593133703));
#22619=CARTESIAN_POINT('Origin',(275.045504100673,188.546028205476,260.073593133703));
#22620=CARTESIAN_POINT('',(281.319563895274,178.316845750668,260.073593133703));
#22621=CARTESIAN_POINT('Origin',(275.045504100673,188.546028205476,260.073593133703));
#22622=CARTESIAN_POINT('',(303.48279254736,191.910641972304,260.073593133703));
#22623=CARTESIAN_POINT('',(303.48279254736,191.910641972304,260.073593133703));
#22624=CARTESIAN_POINT('Origin',(297.208732752758,202.139824427113,260.073593133703));
#22625=CARTESIAN_POINT('',(278.513621142497,182.891634853029,250.073593133703));
#22626=CARTESIAN_POINT('Origin',(275.045504100673,188.546028205476,260.073593133703));
#22627=CARTESIAN_POINT('',(275.045504100673,188.546028205476,248.073593133703));
#22628=CARTESIAN_POINT('Origin',(275.045504100673,188.546028205476,260.073593133703));
#22629=CARTESIAN_POINT('',(239.243365508842,166.586818924372,248.073593133703));
#22630=CARTESIAN_POINT('',(297.208732752758,202.139824427113,248.073593133703));
#22631=CARTESIAN_POINT('',(236.629173927758,170.848978280542,249.164881019068));
#22632=CARTESIAN_POINT('Origin',(239.243365508842,166.586818924372,260.073593133703));
#22633=CARTESIAN_POINT('',(255.058804871617,182.152775729169,249.164881019068));
#22634=CARTESIAN_POINT('',(236.629173927758,170.848978280542,249.164881019068));
#22635=CARTESIAN_POINT('Ctrl Pts',(255.058804871617,182.152775729169,249.164881019068));
#22636=CARTESIAN_POINT('Ctrl Pts',(255.102027325485,182.179286182221,249.164881019113));
#22637=CARTESIAN_POINT('Ctrl Pts',(255.142563428073,182.208749139151,249.166674552376));
#22638=CARTESIAN_POINT('Ctrl Pts',(255.179508383441,182.24215669622,249.170886992558));
#22639=CARTESIAN_POINT('Ctrl Pts',(255.1926006349,182.253995393369,249.172379762696));
#22640=CARTESIAN_POINT('Ctrl Pts',(255.205242003714,182.26632930192,249.174176678126));
#22641=CARTESIAN_POINT('Ctrl Pts',(255.217392602471,182.279201956245,249.176307129975));
#22642=CARTESIAN_POINT('Ctrl Pts',(255.249844358091,182.313582174103,249.181997129631));
#22643=CARTESIAN_POINT('Ctrl Pts',(255.278272607663,182.352497583317,249.190460078823));
#22644=CARTESIAN_POINT('Ctrl Pts',(255.299732473223,182.393719901414,249.201635214537));
#22645=CARTESIAN_POINT('Ctrl Pts',(255.308981574346,182.411486526629,249.20645164547));
#22646=CARTESIAN_POINT('Ctrl Pts',(255.316936407192,182.429681419483,249.211772506003));
#22647=CARTESIAN_POINT('Ctrl Pts',(255.323361884996,182.448125072141,249.217595537228));
#22648=CARTESIAN_POINT('Origin',(256.292002933523,177.043585248707,248.073593133703));
#22649=CARTESIAN_POINT('',(225.604455569097,158.221405864903,250.073593133703));
#22650=CARTESIAN_POINT('',(256.292002933523,177.043585248707,250.073593133703));
#22651=CARTESIAN_POINT('',(239.243365508842,166.586818924372,248.073593133703));
#22652=CARTESIAN_POINT('',(225.604455569097,158.221405864903,248.073593133703));
#22653=CARTESIAN_POINT('',(256.292002933523,177.043585248707,248.073593133703));
#22654=CARTESIAN_POINT('',(225.604455569097,158.221405864903,248.073593133703));
#22655=CARTESIAN_POINT('Origin',(256.292002933523,177.043585248707,272.073593133703));
#22656=CARTESIAN_POINT('',(239.243365508842,166.586818924372,270.073593133703));
#22657=CARTESIAN_POINT('',(225.604455569097,158.221405864903,270.073593133703));
#22658=CARTESIAN_POINT('',(256.292002933523,177.043585248707,270.073593133703));
#22659=CARTESIAN_POINT('',(225.604455569097,158.221405864903,272.073593133703));
#22660=CARTESIAN_POINT('',(225.604455569097,158.221405864903,272.073593133703));
#22661=CARTESIAN_POINT('',(256.292002933523,177.043585248707,272.073593133703));
#22662=CARTESIAN_POINT('Origin',(275.045504100673,188.546028205476,230.073593133703));
#22663=CARTESIAN_POINT('',(275.045504100673,188.546028205476,270.073593133703));
#22664=CARTESIAN_POINT('',(275.045504100673,188.546028205476,250.073593133703));
#22665=CARTESIAN_POINT('Origin',(297.208732752758,202.139824427113,260.073593133703));
#22666=CARTESIAN_POINT('Origin',(275.045504100673,188.546028205476,248.073593133703));
#22667=CARTESIAN_POINT('',(289.684976954742,164.677935810923,248.073593133703));
#22668=CARTESIAN_POINT('',(275.045504100673,188.546028205476,248.073593133703));
#22669=CARTESIAN_POINT('',(289.684976954742,164.677935810923,250.073593133703));
#22670=CARTESIAN_POINT('',(275.045504100673,188.546028205476,250.073593133703));
#22671=CARTESIAN_POINT('',(289.684976954742,164.677935810923,248.073593133703));
#22672=CARTESIAN_POINT('Origin',(270.931475787593,153.175492854154,248.073593133703));
#22673=CARTESIAN_POINT('',(268.374180173891,151.606977905503,250.073593133703));
#22674=CARTESIAN_POINT('',(270.931475787593,153.175492854154,250.073593133703));
#22675=CARTESIAN_POINT('',(268.374180173891,151.606977905503,248.073593133703));
#22676=CARTESIAN_POINT('',(268.374180173891,151.606977905503,248.073593133703));
#22677=CARTESIAN_POINT('',(270.931475787593,153.175492854154,248.073593133703));
#22678=CARTESIAN_POINT('Origin',(263.296036423484,150.278120398498,248.073593133703));
#22679=CARTESIAN_POINT('',(235.015545260999,142.87763218269,250.073593133703));
#22680=CARTESIAN_POINT('',(263.296036423484,150.278120398498,250.073593133703));
#22681=CARTESIAN_POINT('',(235.015545260999,142.87763218269,248.073593133703));
#22682=CARTESIAN_POINT('',(235.015545260999,142.87763218269,248.073593133703));
#22683=CARTESIAN_POINT('',(263.296036423484,150.278120398498,248.073593133703));
#22684=CARTESIAN_POINT('Origin',(225.604455569097,158.221405864903,248.073593133703));
#22685=CARTESIAN_POINT('',(225.604455569097,158.221405864903,250.073593133703));
#22686=CARTESIAN_POINT('',(225.604455569097,158.221405864903,248.073593133703));
#22687=CARTESIAN_POINT('Origin',(256.292002933523,177.043585248707,248.073593133703));
#22688=CARTESIAN_POINT('Origin',(256.292002933523,177.043585248707,250.073593133703));
#22689=CARTESIAN_POINT('Origin',(275.045504100673,188.546028205476,272.073593133703));
#22690=CARTESIAN_POINT('',(289.684976954742,164.677935810923,272.073593133703));
#22691=CARTESIAN_POINT('',(275.045504100673,188.546028205476,272.073593133703));
#22692=CARTESIAN_POINT('',(289.684976954742,164.677935810923,270.073593133703));
#22693=CARTESIAN_POINT('',(289.684976954742,164.677935810923,272.073593133703));
#22694=CARTESIAN_POINT('',(275.045504100673,188.546028205476,270.073593133703));
#22695=CARTESIAN_POINT('Origin',(270.931475787593,153.175492854154,272.073593133703));
#22696=CARTESIAN_POINT('',(268.374180173891,151.606977905503,270.073593133703));
#22697=CARTESIAN_POINT('',(270.931475787593,153.175492854154,270.073593133703));
#22698=CARTESIAN_POINT('',(268.374180173891,151.606977905503,272.073593133703));
#22699=CARTESIAN_POINT('',(270.931475787593,153.175492854154,272.073593133703));
#22700=CARTESIAN_POINT('',(268.374180173891,151.606977905503,272.073593133703));
#22701=CARTESIAN_POINT('Origin',(225.604455569097,158.221405864903,272.073593133703));
#22702=CARTESIAN_POINT('',(235.015545260999,142.87763218269,270.073593133703));
#22703=CARTESIAN_POINT('',(225.604455569097,158.221405864903,270.073593133703));
#22704=CARTESIAN_POINT('',(235.015545260999,142.87763218269,272.073593133703));
#22705=CARTESIAN_POINT('',(235.015545260999,142.87763218269,272.073593133703));
#22706=CARTESIAN_POINT('',(225.604455569097,158.221405864903,272.073593133703));
#22707=CARTESIAN_POINT('Origin',(263.296036423484,150.278120398498,272.073593133703));
#22708=CARTESIAN_POINT('',(263.296036423484,150.278120398498,270.073593133703));
#22709=CARTESIAN_POINT('',(263.296036423484,150.278120398498,272.073593133703));
#22710=CARTESIAN_POINT('Origin',(256.292002933523,177.043585248707,272.073593133703));
#22711=CARTESIAN_POINT('Origin',(256.292002933523,177.043585248707,270.073593133703));
#22712=CARTESIAN_POINT('Origin',(249.999939717625,149.049376857752,260.073593133703));
#22713=CARTESIAN_POINT('Origin',(267.048577142306,159.506143182087,260.073593133703));
#22714=CARTESIAN_POINT('Origin',(249.999939717625,149.049376857752,260.073593133703));
#22715=CARTESIAN_POINT('Origin',(240.326199116368,164.821374714051,260.073593133703));
#22716=CARTESIAN_POINT('Ctrl Pts',(255.058804869969,182.152775728158,270.982305248339));
#22717=CARTESIAN_POINT('Ctrl Pts',(254.922595243703,182.147186996158,270.939231074838));
#22718=CARTESIAN_POINT('Ctrl Pts',(254.792319846723,182.1678785851,270.882674845301));
#22719=CARTESIAN_POINT('Ctrl Pts',(254.547149308436,182.228970127669,270.760014729386));
#22720=CARTESIAN_POINT('Ctrl Pts',(254.430102458011,182.270513662175,270.692574498549));
#22721=CARTESIAN_POINT('Ctrl Pts',(254.091846405705,182.411381584387,270.478647373104));
#22722=CARTESIAN_POINT('Ctrl Pts',(253.888226908793,182.52392263632,270.324232289594));
#22723=CARTESIAN_POINT('Ctrl Pts',(253.503176846748,182.759323529108,269.997439492304));
#22724=CARTESIAN_POINT('Ctrl Pts',(253.322509839,182.883112909143,269.824845969452));
#22725=CARTESIAN_POINT('Ctrl Pts',(252.978070665713,183.133913082514,269.462735650107));
#22726=CARTESIAN_POINT('Ctrl Pts',(252.814019303634,183.261450177997,269.272569866411));
#22727=CARTESIAN_POINT('Ctrl Pts',(252.349393784202,183.637467244233,268.685694556367));
#22728=CARTESIAN_POINT('Ctrl Pts',(252.073664492895,183.880694398784,268.270651629051));
#22729=CARTESIAN_POINT('Ctrl Pts',(251.574095308201,184.338327118907,267.395153694069));
#22730=CARTESIAN_POINT('Ctrl Pts',(251.350598392334,184.553055890188,266.934666983117));
#22731=CARTESIAN_POINT('Ctrl Pts',(251.050673609181,184.84821394174,266.209201808336));
#22732=CARTESIAN_POINT('Ctrl Pts',(250.956756662856,184.942020874301,265.961675454384));
#22733=CARTESIAN_POINT('Ctrl Pts',(250.782916004701,185.117468763908,265.462143203401));
#22734=CARTESIAN_POINT('Ctrl Pts',(250.702618023797,185.199479981665,265.20926576918));
#22735=CARTESIAN_POINT('Ctrl Pts',(250.480600808949,185.428075012049,264.44146848943));
#22736=CARTESIAN_POINT('Ctrl Pts',(250.357646619975,185.557264701136,263.917422833903));
#22737=CARTESIAN_POINT('Ctrl Pts',(250.159716763548,185.766878090088,262.844897070672));
#22738=CARTESIAN_POINT('Ctrl Pts',(250.084593037062,185.847495973639,262.293315498942));
#22739=CARTESIAN_POINT('Ctrl Pts',(249.98515941521,185.95447401283,261.184983142805));
#22740=CARTESIAN_POINT('Ctrl Pts',(249.960387400451,185.981329584333,260.62741827262));
#22741=CARTESIAN_POINT('Ctrl Pts',(249.96100832076,185.98065816754,258.945148252925));
#22742=CARTESIAN_POINT('Ctrl Pts',(250.059575673001,185.872958537603,257.848516427325));
#22743=CARTESIAN_POINT('Ctrl Pts',(250.355456958999,185.559569730516,256.239858184419));
#22744=CARTESIAN_POINT('Ctrl Pts',(250.480425610475,185.42824964895,255.706112477511));
#22745=CARTESIAN_POINT('Ctrl Pts',(250.777739784718,185.122138321099,254.678340409923));
#22746=CARTESIAN_POINT('Ctrl Pts',(250.949992239702,184.947355826575,254.182401072184));
#22747=CARTESIAN_POINT('Ctrl Pts',(251.344711962776,184.558789117574,253.225886058467));
#22748=CARTESIAN_POINT('Ctrl Pts',(251.567066041168,184.344908180937,252.765302871011));
#22749=CARTESIAN_POINT('Ctrl Pts',(252.070625488688,183.883339233532,251.880927869941));
#22750=CARTESIAN_POINT('Ctrl Pts',(252.350194703928,183.63679940324,251.460417476297));
#22751=CARTESIAN_POINT('Ctrl Pts',(252.814261793661,183.261263785637,250.874341464003));
#22752=CARTESIAN_POINT('Ctrl Pts',(252.976797851985,183.134875023001,250.685864335876));
#22753=CARTESIAN_POINT('Ctrl Pts',(253.321579334035,182.883755518574,250.323243418964));
#22754=CARTESIAN_POINT('Ctrl Pts',(253.503980821481,182.758747305024,250.148944925558));
#22755=CARTESIAN_POINT('Ctrl Pts',(253.890944404526,182.522346778811,249.820768240594));
#22756=CARTESIAN_POINT('Ctrl Pts',(254.096402914617,182.409199663039,249.665403438688));
#22757=CARTESIAN_POINT('Ctrl Pts',(254.432638579187,182.26960273328,249.45313743041));
#22758=CARTESIAN_POINT('Ctrl Pts',(254.548686887323,182.228477031682,249.386324330007));
#22759=CARTESIAN_POINT('Ctrl Pts',(254.793947631671,182.167584364359,249.263775994265));
#22760=CARTESIAN_POINT('Ctrl Pts',(254.9238364217,182.147237922157,249.207562689353));
#22761=CARTESIAN_POINT('Ctrl Pts',(255.058804869969,182.152775728158,249.164881019068));
#22762=CARTESIAN_POINT('Origin',(240.326199116368,164.821374714051,260.073593133703));
#22763=CARTESIAN_POINT('Origin',(239.243365508842,166.586818924372,260.073593133703));
#22764=CARTESIAN_POINT('Origin',(256.292002933523,177.043585248707,260.073593133703));
#22765=CARTESIAN_POINT('Origin',(257.996866675991,178.089261881141,260.073593133703));
#22766=CARTESIAN_POINT('Ctrl Pts',(255.32336188472,182.448125072297,249.217595537359));
#22767=CARTESIAN_POINT('Ctrl Pts',(255.305592473701,182.437226220217,249.217595537395));
#22768=CARTESIAN_POINT('Ctrl Pts',(255.286198795864,182.43009894237,249.219874591516));
#22769=CARTESIAN_POINT('Ctrl Pts',(255.266403935544,182.425927343183,249.223717258111));
#22770=CARTESIAN_POINT('Ctrl Pts',(255.251968219503,182.422885138271,249.22651958371));
#22771=CARTESIAN_POINT('Ctrl Pts',(255.237318898632,182.421415083184,249.230152526266));
#22772=CARTESIAN_POINT('Ctrl Pts',(255.222924497431,182.421205660522,249.23432258769));
#22773=CARTESIAN_POINT('Ctrl Pts',(255.203424097226,182.420921951205,249.239971858231));
#22774=CARTESIAN_POINT('Ctrl Pts',(255.184565977027,182.422652171011,249.246434572775));
#22775=CARTESIAN_POINT('Ctrl Pts',(255.166141185898,182.425740259873,249.253443856627));
#22776=CARTESIAN_POINT('Ctrl Pts',(255.152316064946,182.42805742058,249.258703302791));
#22777=CARTESIAN_POINT('Ctrl Pts',(255.138735222325,182.431138529906,249.264271900505));
#22778=CARTESIAN_POINT('Ctrl Pts',(255.125314763442,182.43469985398,249.270053972538));
#22779=CARTESIAN_POINT('Ctrl Pts',(255.098342238399,182.441857426132,249.281674818298));
#22780=CARTESIAN_POINT('Ctrl Pts',(255.072193027228,182.450958116289,249.294100019898));
#22781=CARTESIAN_POINT('Ctrl Pts',(255.046747612105,182.461389632585,249.307045409399));
#22782=CARTESIAN_POINT('Ctrl Pts',(255.018207282478,182.47308992956,249.321565340857));
#22783=CARTESIAN_POINT('Ctrl Pts',(254.99055223487,182.486464125929,249.336740338357));
#22784=CARTESIAN_POINT('Ctrl Pts',(254.963629642091,182.50062736719,249.352228706564));
#22785=CARTESIAN_POINT('Ctrl Pts',(254.958836407747,182.503148956956,249.354986218778));
#22786=CARTESIAN_POINT('Ctrl Pts',(254.954066429165,182.505695517326,249.357753784772));
#22787=CARTESIAN_POINT('Ctrl Pts',(254.949318892957,182.508262007514,249.360529620813));
#22788=CARTESIAN_POINT('Ctrl Pts',(254.913127437292,182.527826895861,249.381690396129));
#22789=CARTESIAN_POINT('Ctrl Pts',(254.878128477634,182.548688694715,249.403418625613));
#22790=CARTESIAN_POINT('Ctrl Pts',(254.844070018945,182.570521714466,249.425585370033));
#22791=CARTESIAN_POINT('Ctrl Pts',(254.80655594336,182.594569941682,249.450001182071));
#22792=CARTESIAN_POINT('Ctrl Pts',(254.770182649824,182.619796322315,249.474949455971));
#22793=CARTESIAN_POINT('Ctrl Pts',(254.734633012517,182.645744317309,249.500318724675));
#22794=CARTESIAN_POINT('Ctrl Pts',(254.704026539747,182.668084252745,249.522160405508));
#22795=CARTESIAN_POINT('Ctrl Pts',(254.67403095503,182.690958613402,249.544315530662));
#22796=CARTESIAN_POINT('Ctrl Pts',(254.644455404621,182.714066428366,249.566739565019));
#22797=CARTESIAN_POINT('Ctrl Pts',(254.590341043457,182.756346779108,249.607768802926));
#22798=CARTESIAN_POINT('Ctrl Pts',(254.537722157117,182.799604455555,249.649719683728));
#22799=CARTESIAN_POINT('Ctrl Pts',(254.486359613436,182.843564713015,249.692468853766));
#22800=CARTESIAN_POINT('Ctrl Pts',(254.432095924541,182.890008007361,249.737632654023));
#22801=CARTESIAN_POINT('Ctrl Pts',(254.379234258228,182.937235353287,249.783688222526));
#22802=CARTESIAN_POINT('Ctrl Pts',(254.327512963319,182.984905076776,249.830544503696));
#22803=CARTESIAN_POINT('Ctrl Pts',(254.271481709556,183.036547139845,249.881305339928));
#22804=CARTESIAN_POINT('Ctrl Pts',(254.216788466965,183.088708348173,249.933006591772));
#22805=CARTESIAN_POINT('Ctrl Pts',(254.163128675427,183.140935448316,249.985582995045));
#22806=CARTESIAN_POINT('Ctrl Pts',(254.148390615218,183.155280009194,250.000023494621));
#22807=CARTESIAN_POINT('Ctrl Pts',(254.133730683178,183.169629439894,250.014530251569));
#22808=CARTESIAN_POINT('Ctrl Pts',(254.119142948937,183.183974129141,250.02910240567));
#22809=CARTESIAN_POINT('Ctrl Pts',(254.037485369745,183.26427121838,250.110672772103));
#22810=CARTESIAN_POINT('Ctrl Pts',(253.958095813474,183.344700205996,250.194375829466));
#22811=CARTESIAN_POINT('Ctrl Pts',(253.880756017281,183.424975212899,250.280039742912));
#22812=CARTESIAN_POINT('Ctrl Pts',(253.798855156596,183.50998438645,250.370755630284));
#22813=CARTESIAN_POINT('Ctrl Pts',(253.719252476785,183.594820876681,250.463671450877));
#22814=CARTESIAN_POINT('Ctrl Pts',(253.641713921974,183.67913063593,250.558639388367));
#22815=CARTESIAN_POINT('Ctrl Pts',(253.556712663608,183.77155479377,250.662747521549));
#22816=CARTESIAN_POINT('Ctrl Pts',(253.474191353476,183.863346039261,250.769322888701));
#22817=CARTESIAN_POINT('Ctrl Pts',(253.393880298491,183.954020152393,250.878219862291));
#22818=CARTESIAN_POINT('Ctrl Pts',(253.340219189988,184.014605502991,250.950981106886));
#22819=CARTESIAN_POINT('Ctrl Pts',(253.287545690091,184.074691736403,251.024779800913));
#22820=CARTESIAN_POINT('Ctrl Pts',(253.2357893457,184.13413038318,251.099579228695));
#22821=CARTESIAN_POINT('Ctrl Pts',(253.152688209842,184.229566394342,251.219678850939));
#22822=CARTESIAN_POINT('Ctrl Pts',(253.071947254646,184.323639013818,251.342475391721));
#22823=CARTESIAN_POINT('Ctrl Pts',(252.993394165095,184.416208073786,251.467962021102));
#22824=CARTESIAN_POINT('Ctrl Pts',(252.945942178244,184.47212676319,251.543765403519));
#22825=CARTESIAN_POINT('Ctrl Pts',(252.899289102358,184.527496308855,251.620551219808));
#22826=CARTESIAN_POINT('Ctrl Pts',(252.853402096841,184.582281191483,251.698323923814));
#22827=CARTESIAN_POINT('Ctrl Pts',(252.792477402011,184.655019698123,251.8015836202));
#22828=CARTESIAN_POINT('Ctrl Pts',(252.732831847409,184.726825457145,251.906717635845));
#22829=CARTESIAN_POINT('Ctrl Pts',(252.674625268463,184.797384011339,252.013355098741));
#22830=CARTESIAN_POINT('Ctrl Pts',(252.616418689517,184.867942565532,252.119992561637));
#22831=CARTESIAN_POINT('Ctrl Pts',(252.559651171105,184.937253744578,252.228133237983));
#22832=CARTESIAN_POINT('Ctrl Pts',(252.504457767201,185.005044677865,252.337370321838));
#22833=CARTESIAN_POINT('Ctrl Pts',(252.42657046849,185.100709237347,252.491522462831));
#22834=CARTESIAN_POINT('Ctrl Pts',(252.351675222557,185.193488613487,252.648102763049));
#22835=CARTESIAN_POINT('Ctrl Pts',(252.279627173469,185.283369929189,252.8070552405));
#22836=CARTESIAN_POINT('Ctrl Pts',(252.205887223038,185.375361924093,252.969740392375));
#22837=CARTESIAN_POINT('Ctrl Pts',(252.135129557654,185.464318441126,253.134910972967));
#22838=CARTESIAN_POINT('Ctrl Pts',(252.067226908187,185.550195451901,253.302543574781));
#22839=CARTESIAN_POINT('Ctrl Pts',(252.013418480972,185.618247389785,253.435381493836));
#22840=CARTESIAN_POINT('Ctrl Pts',(251.961403419595,185.684364966429,253.569766278894));
#22841=CARTESIAN_POINT('Ctrl Pts',(251.911131498665,185.748511641906,253.705698605741));
#22842=CARTESIAN_POINT('Ctrl Pts',(251.845227331299,185.83260497191,253.883899610465));
#22843=CARTESIAN_POINT('Ctrl Pts',(251.782324757381,185.913318714639,254.064750713446));
#22844=CARTESIAN_POINT('Ctrl Pts',(251.722366218587,185.99060689966,254.248259140579));
#22845=CARTESIAN_POINT('Ctrl Pts',(251.662264405385,186.068079769288,254.432206071753));
#22846=CARTESIAN_POINT('Ctrl Pts',(251.605120605634,186.142110878666,254.618823595358));
#22847=CARTESIAN_POINT('Ctrl Pts',(251.550905771698,186.212615651627,254.808139774963));
#22848=CARTESIAN_POINT('Ctrl Pts',(251.515017728347,186.259286980575,254.933459484857));
#22849=CARTESIAN_POINT('Ctrl Pts',(251.480413730466,186.304412307625,255.059962134081));
#22850=CARTESIAN_POINT('Ctrl Pts',(251.447092607203,186.347957341824,255.187659050152));
#22851=CARTESIAN_POINT('Ctrl Pts',(251.413623787562,186.391695390037,255.31592198471));
#22852=CARTESIAN_POINT('Ctrl Pts',(251.381388138616,186.433927793499,255.445645779032));
#22853=CARTESIAN_POINT('Ctrl Pts',(251.350508544363,186.47446346869,255.576380416569));
#22854=CARTESIAN_POINT('Ctrl Pts',(251.321175965177,186.512968375609,255.70056547148));
#22855=CARTESIAN_POINT('Ctrl Pts',(251.293066796372,186.549942577642,255.825662190079));
#22856=CARTESIAN_POINT('Ctrl Pts',(251.266260224554,186.585265045835,255.951266227758));
#22857=CARTESIAN_POINT('Ctrl Pts',(251.264846432393,186.587127970679,255.957890648253));
#22858=CARTESIAN_POINT('Ctrl Pts',(251.263436257508,186.588986310925,255.964516476233));
#22859=CARTESIAN_POINT('Ctrl Pts',(251.262029709513,186.590840052102,255.971143651196));
#22860=CARTESIAN_POINT('Ctrl Pts',(251.22001307173,186.646215319669,256.169111734006));
#22861=CARTESIAN_POINT('Ctrl Pts',(251.181280148853,186.697414865585,256.36803659797));
#22862=CARTESIAN_POINT('Ctrl Pts',(251.14573394388,186.744500799677,256.567896415216));
#22863=CARTESIAN_POINT('Ctrl Pts',(251.133775781622,186.760341062803,256.635131613045));
#22864=CARTESIAN_POINT('Ctrl Pts',(251.122178501551,186.775715462994,256.702472823652));
#22865=CARTESIAN_POINT('Ctrl Pts',(251.110939119017,186.790625402752,256.769919772245));
#22866=CARTESIAN_POINT('Ctrl Pts',(251.07666058089,186.83609862487,256.975623492344));
#22867=CARTESIAN_POINT('Ctrl Pts',(251.045703415176,186.877231614162,257.182305293813));
#22868=CARTESIAN_POINT('Ctrl Pts',(251.01801554753,186.914072166413,257.389953006453));
#22869=CARTESIAN_POINT('Ctrl Pts',(250.988873109874,186.952848120953,257.608509400803));
#22870=CARTESIAN_POINT('Ctrl Pts',(250.963352139096,186.986869307684,257.828136343562));
#22871=CARTESIAN_POINT('Ctrl Pts',(250.941425713081,187.016143062935,258.048838461296));
#22872=CARTESIAN_POINT('Ctrl Pts',(250.92055028519,187.044013640948,258.258961677032));
#22873=CARTESIAN_POINT('Ctrl Pts',(250.902933271537,187.067580711243,258.470060113447));
#22874=CARTESIAN_POINT('Ctrl Pts',(250.888581473397,187.086807478048,258.682145548763));
#22875=CARTESIAN_POINT('Ctrl Pts',(250.874282432124,187.105963567715,258.893451363066));
#22876=CARTESIAN_POINT('Ctrl Pts',(250.863224638294,187.120811223589,259.105737473469));
#22877=CARTESIAN_POINT('Ctrl Pts',(250.855444255506,187.131271651202,259.319014860937));
#22878=CARTESIAN_POINT('Ctrl Pts',(250.847728740891,187.141644866032,259.530514069237));
#22879=CARTESIAN_POINT('Ctrl Pts',(250.843236249268,187.14770366393,259.742988617007));
#22880=CARTESIAN_POINT('Ctrl Pts',(250.842030805421,187.149329638876,259.956440655387));
#22881=CARTESIAN_POINT('Ctrl Pts',(250.841827424176,187.149603971695,259.992454063485));
#22882=CARTESIAN_POINT('Ctrl Pts',(250.841717678375,187.149752023718,260.02849526646));
#22883=CARTESIAN_POINT('Ctrl Pts',(250.841701955889,187.149773109793,260.06456423381));
#22884=CARTESIAN_POINT('Ctrl Pts',(250.841606110561,187.149901651909,260.284443062896));
#22885=CARTESIAN_POINT('Ctrl Pts',(250.845007611412,187.145332323719,260.503797799271));
#22886=CARTESIAN_POINT('Ctrl Pts',(250.851874504217,187.136124450971,260.722610014815));
#22887=CARTESIAN_POINT('Ctrl Pts',(250.858758705094,187.126893369687,260.941973748737));
#22888=CARTESIAN_POINT('Ctrl Pts',(250.869125789004,187.113000327815,261.160792798172));
#22889=CARTESIAN_POINT('Ctrl Pts',(250.882973567754,187.094462308955,261.379050191942));
#22890=CARTESIAN_POINT('Ctrl Pts',(250.890649367219,187.084186717624,261.500029882383));
#22891=CARTESIAN_POINT('Ctrl Pts',(250.899395130637,187.072483214165,261.620836984648));
#22892=CARTESIAN_POINT('Ctrl Pts',(250.909214425574,187.059349078077,261.74146783121));
#22893=CARTESIAN_POINT('Ctrl Pts',(250.92293432421,187.040997555189,261.910017915268));
#22894=CARTESIAN_POINT('Ctrl Pts',(250.938765555668,187.019841072376,262.078357348699));
#22895=CARTESIAN_POINT('Ctrl Pts',(250.956686462005,186.995918549522,262.246081476918));
#22896=CARTESIAN_POINT('Ctrl Pts',(250.974606765734,186.971996831088,262.413799965246));
#22897=CARTESIAN_POINT('Ctrl Pts',(250.994616582585,186.945309301798,262.580902869183));
#22898=CARTESIAN_POINT('Ctrl Pts',(251.016668245256,186.915939341316,262.746993592085));
#22899=CARTESIAN_POINT('Ctrl Pts',(251.03875414947,186.88652377553,262.913342218557));
#22900=CARTESIAN_POINT('Ctrl Pts',(251.062888205982,186.854417515176,263.078675204227));
#22901=CARTESIAN_POINT('Ctrl Pts',(251.088996878786,186.819748071741,263.242606920757));
#22902=CARTESIAN_POINT('Ctrl Pts',(251.096643466719,186.809594244704,263.290618487446));
#22903=CARTESIAN_POINT('Ctrl Pts',(251.104459264335,186.799220839185,263.338509959372));
#22904=CARTESIAN_POINT('Ctrl Pts',(251.112442017969,186.788631750385,263.386271915724));
#22905=CARTESIAN_POINT('Ctrl Pts',(251.146825606285,186.743022066478,263.59199384073));
#22906=CARTESIAN_POINT('Ctrl Pts',(251.184376063794,186.693300712314,263.795768788702));
#22907=CARTESIAN_POINT('Ctrl Pts',(251.225096534777,186.639543062093,263.997613250195));
#22908=CARTESIAN_POINT('Ctrl Pts',(251.265759643961,186.585861138784,264.199173378989));
#22909=CARTESIAN_POINT('Ctrl Pts',(251.309583903252,186.528154160268,264.398809008199));
#22910=CARTESIAN_POINT('Ctrl Pts',(251.356601925706,186.466456182231,264.596524895168));
#22911=CARTESIAN_POINT('Ctrl Pts',(251.385290342217,186.428810675265,264.717162799956));
#22912=CARTESIAN_POINT('Ctrl Pts',(251.415168345009,186.389678556072,264.837085736718));
#22913=CARTESIAN_POINT('Ctrl Pts',(251.446248574714,186.349060370531,264.956291312693));
#22914=CARTESIAN_POINT('Ctrl Pts',(251.507611543227,186.268866225762,265.191643756174));
#22915=CARTESIAN_POINT('Ctrl Pts',(251.573766438657,186.182742940431,265.424589848528));
#22916=CARTESIAN_POINT('Ctrl Pts',(251.64473576945,186.090888515716,265.65451838021));
#22917=CARTESIAN_POINT('Ctrl Pts',(251.716280282574,185.998289642073,265.886310404581));
#22918=CARTESIAN_POINT('Ctrl Pts',(251.792717524411,185.899866376696,266.115035751658));
#22919=CARTESIAN_POINT('Ctrl Pts',(251.874053462935,185.795871094589,266.340075157387));
#22920=CARTESIAN_POINT('Ctrl Pts',(251.886945199337,185.779387854975,266.375743875929));
#22921=CARTESIAN_POINT('Ctrl Pts',(251.899959968139,185.762764733898,266.411320009294));
#22922=CARTESIAN_POINT('Ctrl Pts',(251.913097755267,185.746002848768,266.44680110693));
#22923=CARTESIAN_POINT('Ctrl Pts',(251.977474654705,185.663867388441,266.620663191333));
#22924=CARTESIAN_POINT('Ctrl Pts',(252.044458836526,185.578824893745,266.791326093399));
#22925=CARTESIAN_POINT('Ctrl Pts',(252.114089196345,185.491018016114,266.958844062153));
#22926=CARTESIAN_POINT('Ctrl Pts',(252.183213825263,185.403848886895,267.125145334431));
#22927=CARTESIAN_POINT('Ctrl Pts',(252.254946455527,185.313955174931,267.288347764576));
#22928=CARTESIAN_POINT('Ctrl Pts',(252.329354941905,185.221440043281,267.448484623448));
#22929=CARTESIAN_POINT('Ctrl Pts',(252.387524576895,185.14911534349,267.573673336223));
#22930=CARTESIAN_POINT('Ctrl Pts',(252.447330174334,185.075187810648,267.696988229989));
#22931=CARTESIAN_POINT('Ctrl Pts',(252.508816167603,184.999692362965,267.818433227061));
#22932=CARTESIAN_POINT('Ctrl Pts',(252.581135618947,184.91089507654,267.961276094028));
#22933=CARTESIAN_POINT('Ctrl Pts',(252.655762335573,184.819908038571,268.101520561569));
#22934=CARTESIAN_POINT('Ctrl Pts',(252.732846686904,184.726874324985,268.239179237566));
#22935=CARTESIAN_POINT('Ctrl Pts',(252.811212430181,184.63229408932,268.379126247261));
#22936=CARTESIAN_POINT('Ctrl Pts',(252.892118157875,184.535598533268,268.516401736792));
#22937=CARTESIAN_POINT('Ctrl Pts',(252.975755262267,184.436907602098,268.650984600091));
#22938=CARTESIAN_POINT('Ctrl Pts',(253.05354173932,184.345120351587,268.77615305115));
#22939=CARTESIAN_POINT('Ctrl Pts',(253.133691256943,184.251606716133,268.898992714716));
#22940=CARTESIAN_POINT('Ctrl Pts',(253.216382790853,184.156441034041,269.019449088555));
#22941=CARTESIAN_POINT('Ctrl Pts',(253.222602346838,184.149283248235,269.028509086906));
#22942=CARTESIAN_POINT('Ctrl Pts',(253.228836294106,184.142116107116,269.037555582614));
#22943=CARTESIAN_POINT('Ctrl Pts',(253.23508471398,184.134939637759,269.046588542386));
#22944=CARTESIAN_POINT('Ctrl Pts',(253.306413051232,184.053017225876,269.149703572094));
#22945=CARTESIAN_POINT('Ctrl Pts',(253.379751629605,183.969770389543,269.251215988406));
#22946=CARTESIAN_POINT('Ctrl Pts',(253.455018913012,183.885679746065,269.350694801928));
#22947=CARTESIAN_POINT('Ctrl Pts',(253.520365632475,183.812672624774,269.437061863759));
#22948=CARTESIAN_POINT('Ctrl Pts',(253.587165865471,183.739030223278,269.521896731626));
#22949=CARTESIAN_POINT('Ctrl Pts',(253.655357308654,183.66508985876,269.604937666439));
#22950=CARTESIAN_POINT('Ctrl Pts',(253.721469993782,183.593403503266,269.685447169095));
#22951=CARTESIAN_POINT('Ctrl Pts',(253.788913289867,183.521349913543,269.764328269069));
#22952=CARTESIAN_POINT('Ctrl Pts',(253.857933938861,183.449186383109,269.841586336771));
#22953=CARTESIAN_POINT('Ctrl Pts',(253.923031167831,183.381124927118,269.914452735395));
#22954=CARTESIAN_POINT('Ctrl Pts',(253.989531816038,183.312965555382,269.985875904148));
#22955=CARTESIAN_POINT('Ctrl Pts',(254.057666508963,183.244906879936,270.05582404412));
#22956=CARTESIAN_POINT('Ctrl Pts',(254.077627986578,183.224967673225,270.076316808823));
#22957=CARTESIAN_POINT('Ctrl Pts',(254.097729863561,183.205036996922,270.096682691231));
#22958=CARTESIAN_POINT('Ctrl Pts',(254.117978295483,183.185119561377,270.116920145927));
#22959=CARTESIAN_POINT('Ctrl Pts',(254.168638618129,183.135287371168,270.167553004235));
#22960=CARTESIAN_POINT('Ctrl Pts',(254.220156691413,183.085397762633,270.217392754447));
#22961=CARTESIAN_POINT('Ctrl Pts',(254.272829857711,183.035824074896,270.266425929164));
#22962=CARTESIAN_POINT('Ctrl Pts',(254.322838834282,182.988757806381,270.312979023613));
#22963=CARTESIAN_POINT('Ctrl Pts',(254.373889180299,182.941976341435,270.358805695447));
#22964=CARTESIAN_POINT('Ctrl Pts',(254.426257942816,182.895783796577,270.403857842544));
#22965=CARTESIAN_POINT('Ctrl Pts',(254.474749681505,182.853011030771,270.445574637814));
#22966=CARTESIAN_POINT('Ctrl Pts',(254.524372093986,182.810743225032,270.486627733615));
#22967=CARTESIAN_POINT('Ctrl Pts',(254.575362051097,182.769208050738,270.526939979175));
#22968=CARTESIAN_POINT('Ctrl Pts',(254.597512071361,182.751165184957,270.544451605123));
#22969=CARTESIAN_POINT('Ctrl Pts',(254.619920357463,182.733260383457,270.561822875596));
#22970=CARTESIAN_POINT('Ctrl Pts',(254.642607244695,182.715511376955,270.57904459608));
#22971=CARTESIAN_POINT('Ctrl Pts',(254.677375991624,182.688310169977,270.605437711852));
#22972=CARTESIAN_POINT('Ctrl Pts',(254.712661735147,182.661478290065,270.6314136033));
#22973=CARTESIAN_POINT('Ctrl Pts',(254.74879651668,182.635472037571,270.656922763078));
#22974=CARTESIAN_POINT('Ctrl Pts',(254.781575063799,182.611881271649,270.680062606749));
#22975=CARTESIAN_POINT('Ctrl Pts',(254.815052444963,182.588969919988,270.702818651702));
#22976=CARTESIAN_POINT('Ctrl Pts',(254.849491525827,182.56706552931,270.725118538041));
#22977=CARTESIAN_POINT('Ctrl Pts',(254.881214538541,182.546888647507,270.745659724394));
#22978=CARTESIAN_POINT('Ctrl Pts',(254.913753677733,182.52756625059,270.765814146755));
#22979=CARTESIAN_POINT('Ctrl Pts',(254.947325690666,182.509341768866,270.785489860278));
#22980=CARTESIAN_POINT('Ctrl Pts',(254.974874835784,182.494386785597,270.801635722257));
#22981=CARTESIAN_POINT('Ctrl Pts',(255.003234322111,182.480064149302,270.817544015284));
#22982=CARTESIAN_POINT('Ctrl Pts',(255.032557552846,182.467371520176,270.832831465269));
#22983=CARTESIAN_POINT('Ctrl Pts',(255.057876881517,182.456411989439,270.846031510456));
#22984=CARTESIAN_POINT('Ctrl Pts',(255.083914893497,182.446667929592,270.858769003089));
#22985=CARTESIAN_POINT('Ctrl Pts',(255.110781390828,182.438767974361,270.870757623905));
#22986=CARTESIAN_POINT('Ctrl Pts',(255.115029956242,182.437518705572,270.872653458674));
#22987=CARTESIAN_POINT('Ctrl Pts',(255.119299262443,182.436315516993,270.874530468985));
#22988=CARTESIAN_POINT('Ctrl Pts',(255.123589769808,182.435160851133,270.876387405171));
#22989=CARTESIAN_POINT('Ctrl Pts',(255.145641523356,182.429226259998,270.885931427743));
#22990=CARTESIAN_POINT('Ctrl Pts',(255.168614853771,182.424524354017,270.895088038127));
#22991=CARTESIAN_POINT('Ctrl Pts',(255.192182661757,182.42240360197,270.90314026354));
#22992=CARTESIAN_POINT('Ctrl Pts',(255.202197358502,182.421502428274,270.906561905285));
#22993=CARTESIAN_POINT('Ctrl Pts',(255.212319486848,182.421067151468,270.909783638002));
#22994=CARTESIAN_POINT('Ctrl Pts',(255.222524416932,182.421200143345,270.912747626903));
#22995=CARTESIAN_POINT('Ctrl Pts',(255.241300295314,182.421444832853,270.918201019985));
#22996=CARTESIAN_POINT('Ctrl Pts',(255.260574263975,182.423855159518,270.922749881881));
#22997=CARTESIAN_POINT('Ctrl Pts',(255.27922678993,182.429091333001,270.925735589379));
#22998=CARTESIAN_POINT('Ctrl Pts',(255.294569863377,182.433398470518,270.928191553227));
#22999=CARTESIAN_POINT('Ctrl Pts',(255.309492000005,182.439617991123,270.929590730021));
#23000=CARTESIAN_POINT('Ctrl Pts',(255.323361884753,182.448125072317,270.929590730047));
#23001=CARTESIAN_POINT('Ctrl Pts',(255.69795971203,182.760768310083,270.863289666853));
#23002=CARTESIAN_POINT('Ctrl Pts',(255.542065616723,182.787419934355,270.793196892032));
#23003=CARTESIAN_POINT('Ctrl Pts',(255.379913538211,182.835032555837,270.757496758746));
#23004=CARTESIAN_POINT('Ctrl Pts',(255.788387377274,182.6113076933,270.977299065995));
#23005=CARTESIAN_POINT('Ctrl Pts',(255.630549472211,182.637016714706,270.909459407662));
#23006=CARTESIAN_POINT('Ctrl Pts',(255.466168344799,182.672413168797,270.864172365102));
#23007=CARTESIAN_POINT('Ctrl Pts',(255.619077812391,182.348069925451,271.063276557297));
#23008=CARTESIAN_POINT('Ctrl Pts',(255.520634101689,182.412422779613,270.996082559504));
#23009=CARTESIAN_POINT('Ctrl Pts',(255.41911229268,182.482769694297,270.941201198992));
#23010=CARTESIAN_POINT('Ctrl Pts',(255.309081965699,182.194018031453,271.043748001287));
#23011=CARTESIAN_POINT('Ctrl Pts',(255.284781185601,182.30336100112,270.976399337839));
#23012=CARTESIAN_POINT('Ctrl Pts',(255.256048943706,182.419383189339,270.923589021742));
#23013=CARTESIAN_POINT('Ctrl Pts',(255.227638836467,182.171517318723,271.028894764525));
#23014=CARTESIAN_POINT('Ctrl Pts',(255.220900220453,182.291278840731,270.961419415091));
#23015=CARTESIAN_POINT('Ctrl Pts',(255.209076752236,182.418439019625,270.910193902727));
#23016=CARTESIAN_POINT('Ctrl Pts',(254.992369492328,182.139063052789,270.967594315179));
#23017=CARTESIAN_POINT('Ctrl Pts',(255.033034731904,182.286438498041,270.89962152934));
#23018=CARTESIAN_POINT('Ctrl Pts',(255.065868025329,182.444215095646,270.85481550798));
#23019=CARTESIAN_POINT('Ctrl Pts',(254.845276603423,182.158294666748,270.906629200941));
#23020=CARTESIAN_POINT('Ctrl Pts',(254.911582333463,182.319980569757,270.838166406986));
#23021=CARTESIAN_POINT('Ctrl Pts',(254.967189227365,182.494967621995,270.79962270377));
#23022=CARTESIAN_POINT('Ctrl Pts',(254.575314234875,182.219156544986,270.776054410111));
#23023=CARTESIAN_POINT('Ctrl Pts',(254.686367581278,182.40516109745,270.706733188276));
#23024=CARTESIAN_POINT('Ctrl Pts',(254.779991222184,182.61080632492,270.680873498225));
#23025=CARTESIAN_POINT('Ctrl Pts',(254.449480404597,182.262946994164,270.704357325665));
#23026=CARTESIAN_POINT('Ctrl Pts',(254.579931124656,182.459173024266,270.634591588456));
#23027=CARTESIAN_POINT('Ctrl Pts',(254.689080556251,182.678457051227,270.61544244106));
#23028=CARTESIAN_POINT('Ctrl Pts',(254.208537366376,182.362149671029,270.552986112183));
#23029=CARTESIAN_POINT('Ctrl Pts',(254.374787969265,182.57680023898,270.48243337455));
#23030=CARTESIAN_POINT('Ctrl Pts',(254.511233959241,182.821808313659,270.476716822089));
#23031=CARTESIAN_POINT('Ctrl Pts',(254.095280913377,182.417198764343,270.474272667784));
#23032=CARTESIAN_POINT('Ctrl Pts',(254.277625278501,182.63991040501,270.403355923987));
#23033=CARTESIAN_POINT('Ctrl Pts',(254.425574355397,182.896754769307,270.404307171622));
#23034=CARTESIAN_POINT('Ctrl Pts',(253.769243527662,182.59039034952,270.230560291979));
#23035=CARTESIAN_POINT('Ctrl Pts',(253.996372167823,182.835464225051,270.158425854918));
#23036=CARTESIAN_POINT('Ctrl Pts',(254.175230499608,183.125969043173,270.179232040224));
#23037=CARTESIAN_POINT('Ctrl Pts',(253.570030440553,182.716405639144,270.058020584565));
#23038=CARTESIAN_POINT('Ctrl Pts',(253.823130620869,182.973594173456,269.985397145909));
#23039=CARTESIAN_POINT('Ctrl Pts',(254.017113051129,183.284502373521,270.018746187404));
#23040=CARTESIAN_POINT('Ctrl Pts',(253.193152505323,182.973731799716,269.695353089176));
#23041=CARTESIAN_POINT('Ctrl Pts',(253.494005385797,183.252498852315,269.622233265112));
#23042=CARTESIAN_POINT('Ctrl Pts',(253.712692616096,183.602487682801,269.678924564811));
#23043=CARTESIAN_POINT('Ctrl Pts',(253.015610508868,183.10569901033,269.504802628584));
#23044=CARTESIAN_POINT('Ctrl Pts',(253.338259190744,183.393881117277,269.43160775279));
#23045=CARTESIAN_POINT('Ctrl Pts',(253.566313219562,183.76249158633,269.499192996309));
#23046=CARTESIAN_POINT('Ctrl Pts',(252.510219054762,183.500014386828,268.90971068143));
#23047=CARTESIAN_POINT('Ctrl Pts',(252.892708926363,183.814710175669,268.835653720007));
#23048=CARTESIAN_POINT('Ctrl Pts',(253.144000705384,184.236445869242,268.934147470799));
#23049=CARTESIAN_POINT('Ctrl Pts',(252.21379797866,183.756625851448,268.487768626105));
#23050=CARTESIAN_POINT('Ctrl Pts',(252.630928206058,184.084365475791,268.414865728006));
#23051=CARTESIAN_POINT('Ctrl Pts',(252.888614147946,184.539611307648,268.528724253357));
#23052=CARTESIAN_POINT('Ctrl Pts',(251.678465949766,184.239590353276,267.596296773091));
#23053=CARTESIAN_POINT('Ctrl Pts',(252.156838953501,184.590134712182,267.527194887727));
#23054=CARTESIAN_POINT('Ctrl Pts',(252.420283367909,185.108451280444,267.662745539141));
#23055=CARTESIAN_POINT('Ctrl Pts',(251.440149873111,184.466440448225,267.126721548513));
#23056=CARTESIAN_POINT('Ctrl Pts',(251.945666293451,184.826117950235,267.060380338219));
#23057=CARTESIAN_POINT('Ctrl Pts',(252.207603382145,185.374426340438,267.202149362294));
#23058=CARTESIAN_POINT('Ctrl Pts',(251.120880433865,184.778331207481,266.386173310803));
#23059=CARTESIAN_POINT('Ctrl Pts',(251.662713290358,185.149605958963,266.32613025419));
#23060=CARTESIAN_POINT('Ctrl Pts',(251.919413580121,185.740053888074,266.46935921003));
#23061=CARTESIAN_POINT('Ctrl Pts',(251.020631854738,184.877861632215,266.132433857755));
#23062=CARTESIAN_POINT('Ctrl Pts',(251.573717325274,185.252826583724,266.074271837757));
#23063=CARTESIAN_POINT('Ctrl Pts',(251.828285193104,185.856697231355,266.217256414804));
#23064=CARTESIAN_POINT('Ctrl Pts',(250.835058673596,185.064199897975,265.619443034692));
#23065=CARTESIAN_POINT('Ctrl Pts',(251.408881398008,185.445954511362,265.56525067354));
#23066=CARTESIAN_POINT('Ctrl Pts',(251.658709051878,186.075107733935,265.705670744697));
#23067=CARTESIAN_POINT('Ctrl Pts',(250.749449478807,185.151281700865,265.359658969482));
#23068=CARTESIAN_POINT('Ctrl Pts',(251.332858495523,185.536071698513,265.307631788323));
#23069=CARTESIAN_POINT('Ctrl Pts',(251.580006721225,186.177194952975,265.445667169421));
#23070=CARTESIAN_POINT('Ctrl Pts',(250.512931393725,185.393971069805,264.570646581531));
#23071=CARTESIAN_POINT('Ctrl Pts',(251.122429833441,185.787492196982,264.524265624361));
#23072=CARTESIAN_POINT('Ctrl Pts',(251.361638634229,186.461806439964,264.653490036942));
#23073=CARTESIAN_POINT('Ctrl Pts',(250.382202619427,185.531072224838,264.031800236087));
#23074=CARTESIAN_POINT('Ctrl Pts',(251.006472559572,185.928841924294,263.990771434713));
#23075=CARTESIAN_POINT('Ctrl Pts',(251.239619961047,186.622748967039,264.109175603941));
#23076=CARTESIAN_POINT('Ctrl Pts',(250.171863847949,185.753517650536,262.928444837571));
#23077=CARTESIAN_POINT('Ctrl Pts',(250.819578279876,186.158438332912,262.898037648395));
#23078=CARTESIAN_POINT('Ctrl Pts',(251.042392746885,186.884097112,262.989762845941));
#23079=CARTESIAN_POINT('Ctrl Pts',(250.092065247842,185.839108858332,262.360616500679));
#23080=CARTESIAN_POINT('Ctrl Pts',(250.748811398794,186.246530121276,262.336402006455));
#23081=CARTESIAN_POINT('Ctrl Pts',(250.966993715978,186.984782734557,262.411264016072));
#23082=CARTESIAN_POINT('Ctrl Pts',(249.986394459609,185.952757018574,261.21805700291));
#23083=CARTESIAN_POINT('Ctrl Pts',(250.654929677702,186.363693623886,261.205549911323));
#23084=CARTESIAN_POINT('Ctrl Pts',(250.86699061522,187.118523637578,261.244648862485));
#23085=CARTESIAN_POINT('Ctrl Pts',(249.960109375638,185.981256709722,260.643179975231));
#23086=CARTESIAN_POINT('Ctrl Pts',(250.631625253859,186.393001588752,260.637234645382));
#23087=CARTESIAN_POINT('Ctrl Pts',(250.842000505805,187.152093026429,260.656413628318));
#23088=CARTESIAN_POINT('Ctrl Pts',(249.960905241707,185.980396154132,258.908570805387));
#23089=CARTESIAN_POINT('Ctrl Pts',(250.632332281791,186.392114734583,258.920748434052));
#23090=CARTESIAN_POINT('Ctrl Pts',(250.84275598636,187.151079700571,258.881502896051));
#23091=CARTESIAN_POINT('Ctrl Pts',(250.065633252246,185.865882874739,257.778333653513));
#23092=CARTESIAN_POINT('Ctrl Pts',(250.724653494205,186.275071296267,257.806485704709));
#23093=CARTESIAN_POINT('Ctrl Pts',(250.942775774683,187.016113768484,257.725189584552));
#23094=CARTESIAN_POINT('Ctrl Pts',(250.380864499977,185.532477343041,256.121241766934));
#23095=CARTESIAN_POINT('Ctrl Pts',(251.00528385278,185.93029262334,256.162216522362));
#23096=CARTESIAN_POINT('Ctrl Pts',(251.238370010026,186.624398843282,256.043933065562));
#23097=CARTESIAN_POINT('Ctrl Pts',(250.514011721928,185.392842215478,255.57225813953));
#23098=CARTESIAN_POINT('Ctrl Pts',(251.123387551199,185.786328698607,255.618684551377));
#23099=CARTESIAN_POINT('Ctrl Pts',(251.362645044373,186.460481651283,255.489375917092));
#23100=CARTESIAN_POINT('Ctrl Pts',(250.830318559901,185.068323104174,254.518436453205));
#23101=CARTESIAN_POINT('Ctrl Pts',(251.404418795496,185.45059063801,254.573829497636));
#23102=CARTESIAN_POINT('Ctrl Pts',(251.654661916545,186.07990581835,254.431367315278));
#23103=CARTESIAN_POINT('Ctrl Pts',(251.01372557053,184.883066549833,254.010308997639));
#23104=CARTESIAN_POINT('Ctrl Pts',(251.567097640648,185.258971787377,254.069913461328));
#23105=CARTESIAN_POINT('Ctrl Pts',(251.82266868169,185.862831131789,253.92454353509));
#23106=CARTESIAN_POINT('Ctrl Pts',(251.435183105815,184.471236242898,253.031245832271));
#23107=CARTESIAN_POINT('Ctrl Pts',(251.941270764064,184.8310916679,253.097487852073));
#23108=CARTESIAN_POINT('Ctrl Pts',(252.203142475808,185.380049794653,252.955669568942));
#23109=CARTESIAN_POINT('Ctrl Pts',(251.673063255092,184.244533938978,252.560299088865));
#23110=CARTESIAN_POINT('Ctrl Pts',(252.152028447736,184.595329145257,252.629402359262));
#23111=CARTESIAN_POINT('Ctrl Pts',(252.415532683477,185.114266209537,252.493606043876));
#23112=CARTESIAN_POINT('Ctrl Pts',(252.214767072122,183.755682726479,251.65739454731));
#23113=CARTESIAN_POINT('Ctrl Pts',(252.631765976759,184.083410260715,251.730354544452));
#23114=CARTESIAN_POINT('Ctrl Pts',(252.88948604426,184.538507962755,251.616471964354));
#23115=CARTESIAN_POINT('Ctrl Pts',(252.513395480913,183.497442401041,251.233479557366));
#23116=CARTESIAN_POINT('Ctrl Pts',(252.895520198024,183.811972357617,251.307525668854));
#23117=CARTESIAN_POINT('Ctrl Pts',(253.146682958596,184.23337465506,251.209228221821));
#23118=CARTESIAN_POINT('Ctrl Pts',(253.016637605481,183.104944858353,250.641303159677));
#23119=CARTESIAN_POINT('Ctrl Pts',(253.339162767622,183.393068983501,250.714493355331));
#23120=CARTESIAN_POINT('Ctrl Pts',(253.567157366365,183.761574936337,250.646975576108));
#23121=CARTESIAN_POINT('Ctrl Pts',(253.193960610691,182.973101659209,250.450914901744));
#23122=CARTESIAN_POINT('Ctrl Pts',(253.494711976584,183.251831639529,250.524039761223));
#23123=CARTESIAN_POINT('Ctrl Pts',(253.713366926182,183.601731584937,250.467392937178));
#23124=CARTESIAN_POINT('Ctrl Pts',(253.573217473954,182.714308793454,250.086240949678));
#23125=CARTESIAN_POINT('Ctrl Pts',(253.825903660531,182.971313112234,250.158863657386));
#23126=CARTESIAN_POINT('Ctrl Pts',(254.019665577714,183.281888396407,250.125707988976));
#23127=CARTESIAN_POINT('Ctrl Pts',(253.773477418047,182.587816240006,249.913093051726));
#23128=CARTESIAN_POINT('Ctrl Pts',(254.0000449561,182.832626574658,249.985218181233));
#23129=CARTESIAN_POINT('Ctrl Pts',(254.178563913084,183.122695807423,249.964674450387));
#23130=CARTESIAN_POINT('Ctrl Pts',(254.100587499649,182.414548019999,249.669137321989));
#23131=CARTESIAN_POINT('Ctrl Pts',(254.282183330116,182.63688758736,249.740038146342));
#23132=CARTESIAN_POINT('Ctrl Pts',(254.429606317529,182.893177505095,249.739400387974));
#23133=CARTESIAN_POINT('Ctrl Pts',(254.214569077146,182.359411089098,249.590185103147));
#23134=CARTESIAN_POINT('Ctrl Pts',(254.379947576733,182.573617767892,249.660717158142));
#23135=CARTESIAN_POINT('Ctrl Pts',(254.515748475552,182.817990681841,249.66678196835));
#23136=CARTESIAN_POINT('Ctrl Pts',(254.454267136741,182.261243106653,249.440057780993));
#23137=CARTESIAN_POINT('Ctrl Pts',(254.583984420675,182.457082712603,249.509806195947));
#23138=CARTESIAN_POINT('Ctrl Pts',(254.69254854312,182.675848723747,249.529212381473));
#23139=CARTESIAN_POINT('Ctrl Pts',(254.579431140785,182.217862721287,249.368887742416));
#23140=CARTESIAN_POINT('Ctrl Pts',(254.689836547022,182.403523225518,249.438195157897));
#23141=CARTESIAN_POINT('Ctrl Pts',(254.782932458239,182.608716259834,249.464266972048));
#23142=CARTESIAN_POINT('Ctrl Pts',(254.850321649343,182.157535534843,249.238378443436));
#23143=CARTESIAN_POINT('Ctrl Pts',(254.915754746099,182.318738837607,249.306825880349));
#23144=CARTESIAN_POINT('Ctrl Pts',(254.970598124639,182.493137486537,249.345587340743));
#23145=CARTESIAN_POINT('Ctrl Pts',(254.998038973668,182.139292856471,249.177802136601));
#23146=CARTESIAN_POINT('Ctrl Pts',(255.037620113726,182.286044696427,249.245759936704));
#23147=CARTESIAN_POINT('Ctrl Pts',(255.069446631777,182.443110220345,249.290752656895));
#23148=CARTESIAN_POINT('Ctrl Pts',(255.229449025207,182.172051550256,249.117980902794));
#23149=CARTESIAN_POINT('Ctrl Pts',(255.222316999038,182.291578833741,249.185453386513));
#23150=CARTESIAN_POINT('Ctrl Pts',(255.210112882693,182.418489907288,249.236712388294));
#23151=CARTESIAN_POINT('Ctrl Pts',(255.309938799049,182.194435982025,249.103380034896));
#23152=CARTESIAN_POINT('Ctrl Pts',(255.28543412136,182.303655305446,249.17072821894));
#23153=CARTESIAN_POINT('Ctrl Pts',(255.25650145862,182.41955152691,249.223544729758));
#23154=CARTESIAN_POINT('Ctrl Pts',(255.616775680461,182.346950242796,249.084067933231));
#23155=CARTESIAN_POINT('Ctrl Pts',(255.518880630488,182.411635590028,249.151263131289));
#23156=CARTESIAN_POINT('Ctrl Pts',(255.417895727355,182.482320258294,249.206127762022));
#23157=CARTESIAN_POINT('Ctrl Pts',(255.791381968628,182.610038677597,249.16820680786));
#23158=CARTESIAN_POINT('Ctrl Pts',(255.633022052011,182.635401590256,249.235995576485));
#23159=CARTESIAN_POINT('Ctrl Pts',(255.468204518472,182.670314620703,249.281404339452));
#23160=CARTESIAN_POINT('Ctrl Pts',(255.694913445605,182.768215148388,249.288918868784));
#23161=CARTESIAN_POINT('Ctrl Pts',(255.539407953281,182.795436716082,249.359305602731));
#23162=CARTESIAN_POINT('Ctrl Pts',(255.37734640349,182.844145577473,249.394812561638));
#23163=CARTESIAN_POINT('',(0.,0.,0.));
#23164=CARTESIAN_POINT('Origin',(636.476617503915,410.22947428139,260.073593133703));
#23165=CARTESIAN_POINT('',(644.455541040985,401.045968459015,260.073593133703));
#23166=CARTESIAN_POINT('',(631.907421451782,421.504333368632,260.073593133703));
#23167=CARTESIAN_POINT('Origin',(638.181481246383,411.275150913823,260.073593133703));
#23168=CARTESIAN_POINT('Origin',(638.181481246383,411.275150913823,260.073593133703));
#23169=CARTESIAN_POINT('',(629.15688107688,422.163520478667,260.073593133703));
#23170=CARTESIAN_POINT('Origin',(630.202557709314,420.458656736199,260.073593133703));
#23171=CARTESIAN_POINT('',(643.79635393095,398.295428084113,260.073593133703));
#23172=CARTESIAN_POINT('Origin',(636.476617503915,410.22947428139,260.073593133703));
#23173=CARTESIAN_POINT('Origin',(636.476617503915,410.22947428139,260.073593133703));
#23174=CARTESIAN_POINT('Origin',(638.181481246383,411.275150913823,260.073593133703));
#23175=CARTESIAN_POINT('',(303.482792547359,191.910641972304,260.073593133703));
#23176=CARTESIAN_POINT('',(644.455541040985,401.045968459015,260.073593133703));
#23177=CARTESIAN_POINT('Origin',(297.208732752758,202.139824427113,260.073593133703));
#23178=CARTESIAN_POINT('Origin',(638.181481246383,411.275150913823,260.073593133703));
#23179=CARTESIAN_POINT('',(304.528469179793,190.205778229836,260.073593133703));
#23180=CARTESIAN_POINT('Origin',(297.208732752758,202.139824427113,260.073593133703));
#23181=CARTESIAN_POINT('',(645.501217673418,399.341104716547,260.073593133703));
#23182=CARTESIAN_POINT('Origin',(297.208732752758,202.139824427113,260.073593133703));
#23183=CARTESIAN_POINT('',(0.,0.,0.));
#23184=CARTESIAN_POINT('Origin',(764.341398189025,488.655221713906,260.073593133703));
#23185=CARTESIAN_POINT('',(754.543818974723,508.454399513489,260.073593133703));
#23186=CARTESIAN_POINT('Origin',(766.046261931493,489.70089834634,260.073593133703));
#23187=CARTESIAN_POINT('',(751.793278599822,509.113586623524,260.073593133703));
#23188=CARTESIAN_POINT('Origin',(752.838955232255,507.408722881056,260.073593133703));
#23189=CARTESIAN_POINT('',(776.889517778227,468.196856804289,260.073593133703));
#23190=CARTESIAN_POINT('Origin',(764.341398189025,488.655221713906,260.073593133703));
#23191=CARTESIAN_POINT('Origin',(764.341398189025,488.655221713906,260.073593133703));
#23192=CARTESIAN_POINT('Origin',(639.886344988851,412.320827546257,260.073593133703));
#23193=CARTESIAN_POINT('',(652.434464578054,391.862462636639,260.073593133703));
#23194=CARTESIAN_POINT('',(627.338225399649,432.779192455874,260.073593133703));
#23195=CARTESIAN_POINT('Origin',(639.886344988851,412.320827546257,260.073593133703));
#23196=CARTESIAN_POINT('Origin',(639.886344988851,412.320827546257,260.073593133703));
#23197=CARTESIAN_POINT('',(626.679038289614,430.028652080973,260.073593133703));
#23198=CARTESIAN_POINT('Origin',(628.383902032082,431.074328713406,260.073593133703));
#23199=CARTESIAN_POINT('Origin',(638.181481246383,411.275150913823,260.073593133703));
#23200=CARTESIAN_POINT('Origin',(766.046261931493,489.70089834634,260.073593133703));
#23201=CARTESIAN_POINT('',(778.594381520695,469.242533436722,260.073593133703));
#23202=CARTESIAN_POINT('Origin',(766.046261931493,489.70089834634,260.073593133703));
#23203=CARTESIAN_POINT('',(720.515222342016,445.350876543623,260.073593133703));
#23204=CARTESIAN_POINT('Origin',(713.195485914981,457.2849227409,260.073593133703));
#23205=CARTESIAN_POINT('',(645.501217673418,399.341104716547,260.073593133703));
#23206=CARTESIAN_POINT('',(773.365998358528,477.766852149063,260.073593133703));
#23207=CARTESIAN_POINT('Origin',(638.181481246383,411.275150913823,260.073593133703));
#23208=CARTESIAN_POINT('Origin',(766.046261931493,489.70089834634,260.073593133703));
#23209=CARTESIAN_POINT('Origin',(638.181481246383,411.275150913823,260.073593133703));
#23210=CARTESIAN_POINT('Origin',(713.195485914981,457.2849227409,260.073593133703));
#23211=CARTESIAN_POINT('',(0.,0.,0.));
#23212=CARTESIAN_POINT('',(0.,0.,0.));
#23213=CARTESIAN_POINT('',(0.,0.,0.));
#23214=CARTESIAN_POINT('',(0.,0.,0.));
#23215=CARTESIAN_POINT('',(0.,0.,0.));
#23216=CARTESIAN_POINT('Origin',(-276.958747352154,52.7397376070391,327.735519388031));
#23217=CARTESIAN_POINT('',(-273.731774309796,57.7980619327321,327.235519388031));
#23218=CARTESIAN_POINT('Origin',(-276.958747352154,52.7397376070391,327.235519388031));
#23219=CARTESIAN_POINT('',(-274.000688729993,57.376534905591,327.735519388031));
#23220=CARTESIAN_POINT('',(-274.000688729993,57.376534905591,327.735519388031));
#23221=CARTESIAN_POINT('Origin',(-276.958747352154,52.7397376070391,327.735519388031));
#23222=CARTESIAN_POINT('Origin',(-276.958747352154,52.7397376070391,178.235519388031));
#23223=CARTESIAN_POINT('',(-273.731774309796,57.7980619327321,178.235519388031));
#23224=CARTESIAN_POINT('',(-280.185720394511,47.6814132813461,178.235519388031));
#23225=CARTESIAN_POINT('Origin',(-276.958747352154,52.7397376070391,178.235519388031));
#23226=CARTESIAN_POINT('Origin',(-276.958747352154,52.7397376070391,178.235519388031));
#23227=CARTESIAN_POINT('',(-279.916805974315,48.1029403084872,177.735519388031));
#23228=CARTESIAN_POINT('',(-280.185720394511,47.6814132813461,178.235519388031));
#23229=CARTESIAN_POINT('Origin',(-276.958747352154,52.7397376070391,177.735519388031));
#23230=CARTESIAN_POINT('Origin',(-276.958747352154,52.7397376070391,327.735519388031));
#23231=CARTESIAN_POINT('',(-273.731774309796,57.7980619327321,327.735519388031));
#23232=CARTESIAN_POINT('Origin',(-276.958747352154,52.7397376070391,327.735519388031));
#23233=CARTESIAN_POINT('Origin',(-276.958747352154,52.7397376070391,177.735519388031));
#23234=CARTESIAN_POINT('',(0.,0.,0.));
#23235=CARTESIAN_POINT('Origin',(-276.958747352154,52.7397376070391,327.323593133701));
#23236=CARTESIAN_POINT('',(-258.632118396215,60.7481501283414,326.723593133701));
#23237=CARTESIAN_POINT('',(-295.285376308092,44.7313250857368,326.723593133701));
#23238=CARTESIAN_POINT('Origin',(-276.958747352154,52.7397376070391,326.723593133701));
#23239=CARTESIAN_POINT('Origin',(-276.958747352154,52.7397376070391,326.723593133701));
#23240=CARTESIAN_POINT('',(-295.83517517677,44.4910727100977,327.323593133701));
#23241=CARTESIAN_POINT('',(-295.83517517677,44.4910727100977,327.323593133701));
#23242=CARTESIAN_POINT('Origin',(-276.958747352154,52.7397376070391,327.323593133701));
#23243=CARTESIAN_POINT('Origin',(-276.958747352154,52.7397376070391,307.923593133701));
#23244=CARTESIAN_POINT('',(-258.632118396215,60.7481501283414,307.923593133701));
#23245=CARTESIAN_POINT('Origin',(-276.958747352154,52.7397376070391,307.923593133701));
#23246=CARTESIAN_POINT('',(-258.082319527537,60.9884025039805,307.323593133701));
#23247=CARTESIAN_POINT('',(-258.632118396215,60.7481501283414,307.923593133701));
#23248=CARTESIAN_POINT('Origin',(-276.958747352154,52.7397376070391,307.323593133701));
#23249=CARTESIAN_POINT('Origin',(-276.958747352154,52.7397376070391,309.323593133701));
#23250=CARTESIAN_POINT('',(-255.883124052824,61.9494120065368,307.323593133701));
#23251=CARTESIAN_POINT('Origin',(-276.958747352154,52.7397376070391,307.323593133701));
#23252=CARTESIAN_POINT('',(-254.05046115723,62.750253258667,309.323593133701));
#23253=CARTESIAN_POINT('Origin',(-255.883124052824,61.9494120065368,309.323593133701));
#23254=CARTESIAN_POINT('',(-299.867033547077,42.7292219554112,309.323593133701));
#23255=CARTESIAN_POINT('Origin',(-276.958747352154,52.7397376070391,309.323593133701));
#23256=CARTESIAN_POINT('Origin',(-276.958747352154,52.7397376070391,309.323593133701));
#23257=CARTESIAN_POINT('Origin',(-276.958747352154,52.7397376070391,309.823593133701));
#23258=CARTESIAN_POINT('',(-260.464781291809,59.9473088762112,311.823593133701));
#23259=CARTESIAN_POINT('Origin',(-276.958747352154,52.7397376070391,311.823593133701));
#23260=CARTESIAN_POINT('',(-258.632118396215,60.7481501283415,309.823593133701));
#23261=CARTESIAN_POINT('Origin',(-260.464781291809,59.9473088762112,309.823593133701));
#23262=CARTESIAN_POINT('Origin',(-276.958747352154,52.7397376070391,309.823593133701));
#23263=CARTESIAN_POINT('Origin',(-276.958747352154,52.7397376070391,325.323593133701));
#23264=CARTESIAN_POINT('',(-299.867033547077,42.7292219554112,325.323593133701));
#23265=CARTESIAN_POINT('',(-254.05046115723,62.750253258667,325.323593133701));
#23266=CARTESIAN_POINT('Origin',(-276.958747352154,52.7397376070391,325.323593133701));
#23267=CARTESIAN_POINT('Origin',(-276.958747352154,52.7397376070391,325.323593133701));
#23268=CARTESIAN_POINT('',(-255.883124052824,61.9494120065368,327.323593133701));
#23269=CARTESIAN_POINT('Origin',(-255.883124052824,61.9494120065368,325.323593133701));
#23270=CARTESIAN_POINT('Origin',(-276.958747352154,52.7397376070391,327.323593133701));
#23271=CARTESIAN_POINT('Origin',(-276.958747352154,52.7397376070391,324.823593133701));
#23272=CARTESIAN_POINT('',(-293.452713412498,45.532166337867,322.823593133701));
#23273=CARTESIAN_POINT('Origin',(-276.958747352154,52.7397376070391,322.823593133701));
#23274=CARTESIAN_POINT('',(-295.285376308092,44.7313250857368,324.823593133701));
#23275=CARTESIAN_POINT('Origin',(-293.452713412498,45.532166337867,324.823593133701));
#23276=CARTESIAN_POINT('',(-258.632118396215,60.7481501283414,324.823593133701));
#23277=CARTESIAN_POINT('Origin',(-276.958747352154,52.7397376070391,324.823593133701));
#23278=CARTESIAN_POINT('Origin',(-276.958747352154,52.7397376070391,324.823593133701));
#23279=CARTESIAN_POINT('Origin',(-276.958747352154,52.7397376070391,327.324593133701));
#23280=CARTESIAN_POINT('',(-272.377090113169,54.7418407373647,327.323593133701));
#23281=CARTESIAN_POINT('Origin',(-276.958747352154,52.7397376070391,327.323593133701));
#23282=CARTESIAN_POINT('',(-272.377090113169,54.7418407373647,307.323593133701));
#23283=CARTESIAN_POINT('',(-272.377090113169,54.7418407373647,327.324593133701));
#23284=CARTESIAN_POINT('Origin',(-276.958747352154,52.7397376070391,307.323593133701));
#23285=CARTESIAN_POINT('Origin',(-276.958747352154,52.7397376070391,307.323593133701));
#23286=CARTESIAN_POINT('',(-290.703719069108,46.7334282160624,311.823593133701));
#23287=CARTESIAN_POINT('Origin',(-276.958747352154,52.7397376070391,311.823593133701));
#23288=CARTESIAN_POINT('',(-283.373067486732,49.9367932245833,307.323593133701));
#23289=CARTESIAN_POINT('',(-283.373067486732,49.9367932245833,307.323593133701));
#23290=CARTESIAN_POINT('Origin',(-276.958747352154,52.7397376070391,307.323593133701));
#23291=CARTESIAN_POINT('Origin',(-276.958747352154,52.7397376070391,317.323593133701));
#23292=CARTESIAN_POINT('',(-258.632118396215,60.7481501283414,317.323593133701));
#23293=CARTESIAN_POINT('Origin',(-276.958747352154,52.7397376070391,322.823593133701));
#23294=CARTESIAN_POINT('',(-263.2137756352,58.7460469980159,322.823593133701));
#23295=CARTESIAN_POINT('Origin',(-276.958747352154,52.7397376070391,322.823593133701));
#23296=CARTESIAN_POINT('',(-270.544427217575,55.5426819894949,327.323593133701));
#23297=CARTESIAN_POINT('',(-263.2137756352,58.7460469980159,322.823593133701));
#23298=CARTESIAN_POINT('Origin',(-276.958747352154,52.7397376070391,327.323593133701));
#23299=CARTESIAN_POINT('Origin',(-276.958747352154,52.7397376070391,317.323593133701));
#23300=CARTESIAN_POINT('',(-258.632118396215,60.7481501283414,317.323593133701));
#23301=CARTESIAN_POINT('Origin',(-276.958747352154,52.7397376070391,307.323593133701));
#23302=CARTESIAN_POINT('',(-299.867033547077,42.7292219554112,307.323593133701));
#23303=CARTESIAN_POINT('Origin',(-276.958747352154,52.7397376070391,307.323593133701));
#23304=CARTESIAN_POINT('Origin',(-276.958747352154,52.7397376070391,327.323593133701));
#23305=CARTESIAN_POINT('Origin',(-284.967159873456,71.0663665629777,322.823593133701));
#23306=CARTESIAN_POINT('Origin',(-284.967159873456,71.0663665629777,311.823593133701));
#23307=CARTESIAN_POINT('Origin',(-276.958747352154,52.7397376070391,327.323593133701));
#23308=CARTESIAN_POINT('Origin',(-276.958747352154,52.7397376070391,307.323593133701));
#23309=CARTESIAN_POINT('',(0.,0.,0.));
#23310=CARTESIAN_POINT('',(0.,0.,0.));
#23311=CARTESIAN_POINT('',(5.6843418860808E-13,-8.88178419700125E-14,-128.500000000001));
#23312=CARTESIAN_POINT('',(0.,0.,0.));
#23313=CARTESIAN_POINT('Origin',(210.55281376718,40.2397376070394,351.055932202117));
#23314=CARTESIAN_POINT('',(229.603651352553,35.4089854465581,354.809519933842));
#23315=CARTESIAN_POINT('',(191.770222858752,45.0704897675207,346.132710459127));
#23316=CARTESIAN_POINT('Origin',(210.686937105653,40.2397376070394,350.471115196485));
#23317=CARTESIAN_POINT('Origin',(210.686937105653,40.2397376070394,350.471115196485));
#23318=CARTESIAN_POINT('',(191.068598092873,45.2154123323351,346.587375322639));
#23319=CARTESIAN_POINT('',(191.068598092873,45.2154123323351,346.587375322639));
#23320=CARTESIAN_POINT('Origin',(210.55281376718,40.2397376070394,351.055932202117));
#23321=CARTESIAN_POINT('Origin',(214.889468377789,40.2397376070394,332.146849019998));
#23322=CARTESIAN_POINT('',(233.806182624689,35.4089854465581,336.485253757356));
#23323=CARTESIAN_POINT('Origin',(214.889468377789,40.2397376070394,332.146849019998));
#23324=CARTESIAN_POINT('',(234.507807390569,35.2640628817436,336.030588893844));
#23325=CARTESIAN_POINT('',(233.806182624689,35.4089854465581,336.485253757356));
#23326=CARTESIAN_POINT('Origin',(215.023591716261,40.2397376070394,331.562032014366));
#23327=CARTESIAN_POINT('Origin',(214.576513921353,40.2397376070394,333.511422033141));
#23328=CARTESIAN_POINT('',(236.777813100197,34.6843726224859,336.551197462327));
#23329=CARTESIAN_POINT('Origin',(215.023591716261,40.2397376070394,331.562032014366));
#23330=CARTESIAN_POINT('',(238.222406729979,34.2012974064378,338.934427954838));
#23331=CARTESIAN_POINT('Origin',(236.330735305289,34.6843726224859,338.500587481102));
#23332=CARTESIAN_POINT('',(190.930621112728,46.278177807641,328.088416111445));
#23333=CARTESIAN_POINT('Origin',(214.576513921353,40.2397376070394,333.511422033141));
#23334=CARTESIAN_POINT('Origin',(214.576513921353,40.2397376070394,333.511422033141));
#23335=CARTESIAN_POINT('Origin',(214.464744472626,40.2397376070394,333.998769537835));
#23336=CARTESIAN_POINT('',(231.042709499928,35.8920606626062,339.852723820232));
#23337=CARTESIAN_POINT('Origin',(214.017666677718,40.2397376070394,335.94815955661));
#23338=CARTESIAN_POINT('',(233.381458719527,35.4089854465581,338.337174275192));
#23339=CARTESIAN_POINT('Origin',(231.489787294837,35.8920606626062,337.903333801457));
#23340=CARTESIAN_POINT('Origin',(214.464744472626,40.2397376070394,333.998769537835));
#23341=CARTESIAN_POINT('Origin',(210.999891562088,40.2397376070394,349.106542183342));
#23342=CARTESIAN_POINT('',(187.353998753463,46.278177807641,343.683536261645));
#23343=CARTESIAN_POINT('',(234.645784370714,34.2012974064378,354.529548105039));
#23344=CARTESIAN_POINT('Origin',(210.999891562088,40.2397376070394,349.106542183342));
#23345=CARTESIAN_POINT('Origin',(210.999891562088,40.2397376070394,349.106542183342));
#23346=CARTESIAN_POINT('',(232.307035151116,34.6843726224859,356.045097650078));
#23347=CARTESIAN_POINT('Origin',(232.754112946024,34.6843726224859,354.095707631303));
#23348=CARTESIAN_POINT('Origin',(210.55281376718,40.2397376070394,351.055932202117));
#23349=CARTESIAN_POINT('Origin',(211.111661010815,40.2397376070394,348.619194678648));
#23350=CARTESIAN_POINT('',(194.533695983513,44.5874145514725,342.765240396252));
#23351=CARTESIAN_POINT('Origin',(211.558738805724,40.2397376070394,346.669804659873));
#23352=CARTESIAN_POINT('',(192.194946763915,45.0704897675207,344.280789941291));
#23353=CARTESIAN_POINT('Origin',(194.086618188605,44.5874145514726,344.714630415027));
#23354=CARTESIAN_POINT('',(230.028375257716,35.4089854465581,352.957599416006));
#23355=CARTESIAN_POINT('Origin',(211.111661010815,40.2397376070394,348.619194678648));
#23356=CARTESIAN_POINT('Origin',(211.111661010815,40.2397376070394,348.619194678648));
#23357=CARTESIAN_POINT('Origin',(210.552590228283,40.2397376070394,351.056906897127));
#23358=CARTESIAN_POINT('',(215.281992328905,39.0320495669191,352.140533386457));
#23359=CARTESIAN_POINT('Origin',(210.55281376718,40.2397376070394,351.055932202117));
#23360=CARTESIAN_POINT('',(219.752770277987,39.0320495669191,332.646633198705));
#23361=CARTESIAN_POINT('',(215.281768790008,39.0320495669191,352.141508081466));
#23362=CARTESIAN_POINT('Origin',(215.023591716261,40.2397376070394,331.562032014366));
#23363=CARTESIAN_POINT('Origin',(215.023591716261,40.2397376070394,331.562032014366));
#23364=CARTESIAN_POINT('',(199.830130992543,43.8628017274004,332.694356003592));
#23365=CARTESIAN_POINT('Origin',(214.017666677718,40.2397376070394,335.94815955661));
#23366=CARTESIAN_POINT('',(208.402741729846,41.9305008632078,330.043590356291));
#23367=CARTESIAN_POINT('',(208.402741729846,41.9305008632078,330.043590356291));
#23368=CARTESIAN_POINT('Origin',(215.023591716261,40.2397376070394,331.562032014366));
#23369=CARTESIAN_POINT('Origin',(212.788202741721,40.2397376070394,341.308982108242));
#23370=CARTESIAN_POINT('',(231.704916988621,35.4089854465581,345.647386845599));
#23371=CARTESIAN_POINT('Origin',(211.558738805724,40.2397376070394,346.669804659873));
#23372=CARTESIAN_POINT('',(225.746274490899,36.6166734866784,349.923608212891));
#23373=CARTESIAN_POINT('Origin',(211.558738805724,40.2397376070394,346.669804659873));
#23374=CARTESIAN_POINT('',(217.173663753595,38.5489743508709,352.574373860192));
#23375=CARTESIAN_POINT('',(225.746274490899,36.6166734866784,349.923608212891));
#23376=CARTESIAN_POINT('Origin',(210.55281376718,40.2397376070394,351.055932202117));
#23377=CARTESIAN_POINT('Origin',(212.788202741721,40.2397376070394,341.308982108242));
#23378=CARTESIAN_POINT('',(231.704916988621,35.4089854465581,345.647386845599));
#23379=CARTESIAN_POINT('Origin',(215.023591716261,40.2397376070394,331.562032014366));
#23380=CARTESIAN_POINT('',(191.377698907636,46.278177807641,326.139026092669));
#23381=CARTESIAN_POINT('Origin',(215.023591716261,40.2397376070394,331.562032014366));
#23382=CARTESIAN_POINT('Origin',(210.55281376718,40.2397376070394,351.055932202117));
#23383=CARTESIAN_POINT('Origin',(216.267248828133,59.6475667892021,347.749665671701));
#23384=CARTESIAN_POINT('Origin',(218.726176700127,59.6475667892021,337.028020568438));
#23385=CARTESIAN_POINT('Origin',(210.55281376718,40.2397376070394,351.055932202117));
#23386=CARTESIAN_POINT('Origin',(215.023591716261,40.2397376070394,331.562032014366));
#23387=CARTESIAN_POINT('Origin',(216.096578424042,40.2397376070391,326.883495969306));
#23388=CARTESIAN_POINT('',(211.320572878043,40.2397376070391,325.78815537178));
#23389=CARTESIAN_POINT('Origin',(216.096578424042,40.2397376070391,326.883495969306));
#23390=CARTESIAN_POINT('',(211.560219659412,40.2397376070391,325.637924149394));
#23391=CARTESIAN_POINT('',(211.320572878043,40.2397376070391,325.78815537178));
#23392=CARTESIAN_POINT('Origin',(216.141286203533,40.2397376070391,326.688556967428));
#23393=CARTESIAN_POINT('Origin',(209.435119279911,40.2397376070391,355.929407249055));
#23394=CARTESIAN_POINT('',(204.703821513403,40.2397376070391,354.639127649653));
#23395=CARTESIAN_POINT('',(214.255832605401,40.2397376070391,356.829808844702));
#23396=CARTESIAN_POINT('Origin',(209.479827059402,40.2397376070391,355.734468247177));
#23397=CARTESIAN_POINT('Origin',(209.479827059402,40.2397376070391,355.734468247177));
#23398=CARTESIAN_POINT('',(214.016185824033,40.2397376070391,356.980040067089));
#23399=CARTESIAN_POINT('',(214.016185824033,40.2397376070391,356.980040067089));
#23400=CARTESIAN_POINT('Origin',(209.435119279911,40.2397376070391,355.929407249055));
#23401=CARTESIAN_POINT('Origin',(219.239377260408,40.2397376070391,313.179973333186));
#23402=CARTESIAN_POINT('',(214.463371714409,40.2397376070391,312.084632735661));
#23403=CARTESIAN_POINT('Origin',(225.888236297409,31.2397376070391,328.923945941969));
#23404=CARTESIAN_POINT('Origin',(209.435119279911,40.2397376070391,355.929407249055));
#23405=CARTESIAN_POINT('Origin',(203.041252647847,101.652237608405,339.0735931337));
#23406=CARTESIAN_POINT('',(202.044552137503,88.2772376084047,343.419499033524));
#23407=CARTESIAN_POINT('',(202.044552137503,88.0272376084047,343.419499033524));
#23408=CARTESIAN_POINT('',(202.044552137504,101.652237608405,343.419499033523));
#23409=CARTESIAN_POINT('',(204.03795315819,87.7772376084047,334.727687233877));
#23410=CARTESIAN_POINT('Ctrl Pts',(202.044552137503,88.2772376084047,343.419499033524));
#23411=CARTESIAN_POINT('Ctrl Pts',(200.244418972999,88.2147376084047,343.006652164516));
#23412=CARTESIAN_POINT('Ctrl Pts',(199.263459426007,88.1522376084047,341.441838976189));
#23413=CARTESIAN_POINT('Ctrl Pts',(198.282499879015,88.0897376084047,339.877025787862));
#23414=CARTESIAN_POINT('Ctrl Pts',(198.695346748023,88.0272376084047,338.076892623358));
#23415=CARTESIAN_POINT('Ctrl Pts',(199.108193617031,87.9647376084047,336.276759458854));
#23416=CARTESIAN_POINT('Ctrl Pts',(200.673006805358,87.9022376084047,335.295799911861));
#23417=CARTESIAN_POINT('Ctrl Pts',(202.237819993686,87.8397376084047,334.314840364869));
#23418=CARTESIAN_POINT('Ctrl Pts',(204.03795315819,87.7772376084047,334.727687233877));
#23419=CARTESIAN_POINT('',(204.03795315819,87.5272376084047,334.727687233877));
#23420=CARTESIAN_POINT('',(204.03795315819,87.6522376084047,334.727687233877));
#23421=CARTESIAN_POINT('Ctrl Pts',(202.044552137503,88.0272376084047,343.419499033524));
#23422=CARTESIAN_POINT('Ctrl Pts',(200.244418972999,87.9647376084047,343.006652164516));
#23423=CARTESIAN_POINT('Ctrl Pts',(199.263459426007,87.9022376084047,341.441838976189));
#23424=CARTESIAN_POINT('Ctrl Pts',(198.282499879015,87.8397376084047,339.877025787862));
#23425=CARTESIAN_POINT('Ctrl Pts',(198.695346748023,87.7772376084047,338.076892623358));
#23426=CARTESIAN_POINT('Ctrl Pts',(199.108193617031,87.7147376084047,336.276759458854));
#23427=CARTESIAN_POINT('Ctrl Pts',(200.673006805358,87.6522376084047,335.295799911861));
#23428=CARTESIAN_POINT('Ctrl Pts',(202.237819993686,87.5897376084047,334.314840364869));
#23429=CARTESIAN_POINT('Ctrl Pts',(204.03795315819,87.5272376084047,334.727687233877));
#23430=CARTESIAN_POINT('Origin',(203.041252647847,101.652237608405,339.0735931337));
#23431=CARTESIAN_POINT('',(202.044552137503,89.2772376084047,343.419499033524));
#23432=CARTESIAN_POINT('',(202.044552137503,89.0272376084047,343.419499033524));
#23433=CARTESIAN_POINT('',(202.044552137504,101.652237608405,343.419499033523));
#23434=CARTESIAN_POINT('Ctrl Pts',(202.044552137503,89.2772376084047,343.419499033524));
#23435=CARTESIAN_POINT('Ctrl Pts',(200.244418972999,89.2147376084047,343.006652164516));
#23436=CARTESIAN_POINT('Ctrl Pts',(199.263459426007,89.1522376084047,341.441838976189));
#23437=CARTESIAN_POINT('Ctrl Pts',(198.282499879015,89.0897376084047,339.877025787862));
#23438=CARTESIAN_POINT('Ctrl Pts',(198.695346748023,89.0272376084047,338.076892623358));
#23439=CARTESIAN_POINT('Ctrl Pts',(199.108193617031,88.9647376084047,336.276759458854));
#23440=CARTESIAN_POINT('Ctrl Pts',(200.673006805358,88.9022376084047,335.295799911861));
#23441=CARTESIAN_POINT('Ctrl Pts',(202.237819993686,88.8397376084047,334.314840364869));
#23442=CARTESIAN_POINT('Ctrl Pts',(204.03795315819,88.7772376084047,334.727687233877));
#23443=CARTESIAN_POINT('Ctrl Pts',(205.838086322694,88.7147376084047,335.140534102886));
#23444=CARTESIAN_POINT('Ctrl Pts',(206.819045869686,88.6522376084047,336.705347291213));
#23445=CARTESIAN_POINT('Ctrl Pts',(207.800005416678,88.5897376084047,338.27016047954));
#23446=CARTESIAN_POINT('Ctrl Pts',(207.38715854767,88.5272376084047,340.070293644044));
#23447=CARTESIAN_POINT('Ctrl Pts',(206.974311678662,88.4647376084047,341.870426808548));
#23448=CARTESIAN_POINT('Ctrl Pts',(205.409498490334,88.4022376084047,342.851386355541));
#23449=CARTESIAN_POINT('Ctrl Pts',(203.844685302007,88.3397376084047,343.832345902533));
#23450=CARTESIAN_POINT('Ctrl Pts',(202.044552137503,88.2772376084047,343.419499033524));
#23451=CARTESIAN_POINT('Ctrl Pts',(202.044552137503,89.0272376084047,343.419499033524));
#23452=CARTESIAN_POINT('Ctrl Pts',(200.244418972999,88.9647376084047,343.006652164516));
#23453=CARTESIAN_POINT('Ctrl Pts',(199.263459426007,88.9022376084047,341.441838976189));
#23454=CARTESIAN_POINT('Ctrl Pts',(198.282499879015,88.8397376084047,339.877025787862));
#23455=CARTESIAN_POINT('Ctrl Pts',(198.695346748023,88.7772376084047,338.076892623358));
#23456=CARTESIAN_POINT('Ctrl Pts',(199.108193617031,88.7147376084047,336.276759458854));
#23457=CARTESIAN_POINT('Ctrl Pts',(200.673006805358,88.6522376084047,335.295799911861));
#23458=CARTESIAN_POINT('Ctrl Pts',(202.237819993686,88.5897376084047,334.314840364869));
#23459=CARTESIAN_POINT('Ctrl Pts',(204.03795315819,88.5272376084047,334.727687233877));
#23460=CARTESIAN_POINT('Ctrl Pts',(205.838086322694,88.4647376084047,335.140534102886));
#23461=CARTESIAN_POINT('Ctrl Pts',(206.819045869686,88.4022376084047,336.705347291213));
#23462=CARTESIAN_POINT('Ctrl Pts',(207.800005416678,88.3397376084047,338.27016047954));
#23463=CARTESIAN_POINT('Ctrl Pts',(207.38715854767,88.2772376084047,340.070293644044));
#23464=CARTESIAN_POINT('Ctrl Pts',(206.974311678662,88.2147376084047,341.870426808548));
#23465=CARTESIAN_POINT('Ctrl Pts',(205.409498490334,88.1522376084047,342.851386355541));
#23466=CARTESIAN_POINT('Ctrl Pts',(203.844685302007,88.0897376084047,343.832345902533));
#23467=CARTESIAN_POINT('Ctrl Pts',(202.044552137503,88.0272376084047,343.419499033524));
#23468=CARTESIAN_POINT('Origin',(203.041252647847,101.652237608405,339.0735931337));
#23469=CARTESIAN_POINT('',(202.044552137503,90.2772376084047,343.419499033524));
#23470=CARTESIAN_POINT('',(202.044552137503,90.0272376084047,343.419499033524));
#23471=CARTESIAN_POINT('',(202.044552137504,101.652237608405,343.419499033523));
#23472=CARTESIAN_POINT('Ctrl Pts',(202.044552137503,90.2772376084047,343.419499033524));
#23473=CARTESIAN_POINT('Ctrl Pts',(200.244418972999,90.2147376084047,343.006652164516));
#23474=CARTESIAN_POINT('Ctrl Pts',(199.263459426007,90.1522376084047,341.441838976189));
#23475=CARTESIAN_POINT('Ctrl Pts',(198.282499879015,90.0897376084047,339.877025787862));
#23476=CARTESIAN_POINT('Ctrl Pts',(198.695346748023,90.0272376084047,338.076892623358));
#23477=CARTESIAN_POINT('Ctrl Pts',(199.108193617031,89.9647376084047,336.276759458854));
#23478=CARTESIAN_POINT('Ctrl Pts',(200.673006805358,89.9022376084047,335.295799911861));
#23479=CARTESIAN_POINT('Ctrl Pts',(202.237819993686,89.8397376084047,334.314840364869));
#23480=CARTESIAN_POINT('Ctrl Pts',(204.03795315819,89.7772376084047,334.727687233877));
#23481=CARTESIAN_POINT('Ctrl Pts',(205.838086322694,89.7147376084047,335.140534102886));
#23482=CARTESIAN_POINT('Ctrl Pts',(206.819045869686,89.6522376084047,336.705347291213));
#23483=CARTESIAN_POINT('Ctrl Pts',(207.800005416678,89.5897376084047,338.27016047954));
#23484=CARTESIAN_POINT('Ctrl Pts',(207.38715854767,89.5272376084047,340.070293644044));
#23485=CARTESIAN_POINT('Ctrl Pts',(206.974311678662,89.4647376084047,341.870426808548));
#23486=CARTESIAN_POINT('Ctrl Pts',(205.409498490334,89.4022376084047,342.851386355541));
#23487=CARTESIAN_POINT('Ctrl Pts',(203.844685302007,89.3397376084047,343.832345902533));
#23488=CARTESIAN_POINT('Ctrl Pts',(202.044552137503,89.2772376084047,343.419499033524));
#23489=CARTESIAN_POINT('Ctrl Pts',(202.044552137503,90.0272376084047,343.419499033524));
#23490=CARTESIAN_POINT('Ctrl Pts',(200.244418972999,89.9647376084047,343.006652164516));
#23491=CARTESIAN_POINT('Ctrl Pts',(199.263459426007,89.9022376084047,341.441838976189));
#23492=CARTESIAN_POINT('Ctrl Pts',(198.282499879015,89.8397376084047,339.877025787862));
#23493=CARTESIAN_POINT('Ctrl Pts',(198.695346748023,89.7772376084047,338.076892623358));
#23494=CARTESIAN_POINT('Ctrl Pts',(199.108193617031,89.7147376084047,336.276759458854));
#23495=CARTESIAN_POINT('Ctrl Pts',(200.673006805358,89.6522376084047,335.295799911861));
#23496=CARTESIAN_POINT('Ctrl Pts',(202.237819993686,89.5897376084047,334.314840364869));
#23497=CARTESIAN_POINT('Ctrl Pts',(204.03795315819,89.5272376084047,334.727687233877));
#23498=CARTESIAN_POINT('Ctrl Pts',(205.838086322694,89.4647376084047,335.140534102886));
#23499=CARTESIAN_POINT('Ctrl Pts',(206.819045869686,89.4022376084047,336.705347291213));
#23500=CARTESIAN_POINT('Ctrl Pts',(207.800005416678,89.3397376084047,338.27016047954));
#23501=CARTESIAN_POINT('Ctrl Pts',(207.38715854767,89.2772376084047,340.070293644044));
#23502=CARTESIAN_POINT('Ctrl Pts',(206.974311678662,89.2147376084047,341.870426808548));
#23503=CARTESIAN_POINT('Ctrl Pts',(205.409498490334,89.1522376084047,342.851386355541));
#23504=CARTESIAN_POINT('Ctrl Pts',(203.844685302007,89.0897376084047,343.832345902533));
#23505=CARTESIAN_POINT('Ctrl Pts',(202.044552137503,89.0272376084047,343.419499033524));
#23506=CARTESIAN_POINT('Origin',(203.041252647847,101.652237608405,339.0735931337));
#23507=CARTESIAN_POINT('',(202.044552137503,91.2772376084047,343.419499033524));
#23508=CARTESIAN_POINT('',(202.044552137503,91.0272376084047,343.419499033524));
#23509=CARTESIAN_POINT('',(202.044552137504,101.652237608405,343.419499033523));
#23510=CARTESIAN_POINT('Ctrl Pts',(202.044552137503,91.2772376084047,343.419499033524));
#23511=CARTESIAN_POINT('Ctrl Pts',(200.244418972999,91.2147376084047,343.006652164516));
#23512=CARTESIAN_POINT('Ctrl Pts',(199.263459426007,91.1522376084047,341.441838976189));
#23513=CARTESIAN_POINT('Ctrl Pts',(198.282499879015,91.0897376084047,339.877025787862));
#23514=CARTESIAN_POINT('Ctrl Pts',(198.695346748023,91.0272376084047,338.076892623358));
#23515=CARTESIAN_POINT('Ctrl Pts',(199.108193617031,90.9647376084047,336.276759458854));
#23516=CARTESIAN_POINT('Ctrl Pts',(200.673006805358,90.9022376084047,335.295799911861));
#23517=CARTESIAN_POINT('Ctrl Pts',(202.237819993686,90.8397376084047,334.314840364869));
#23518=CARTESIAN_POINT('Ctrl Pts',(204.03795315819,90.7772376084047,334.727687233877));
#23519=CARTESIAN_POINT('Ctrl Pts',(205.838086322694,90.7147376084047,335.140534102886));
#23520=CARTESIAN_POINT('Ctrl Pts',(206.819045869686,90.6522376084047,336.705347291213));
#23521=CARTESIAN_POINT('Ctrl Pts',(207.800005416678,90.5897376084047,338.27016047954));
#23522=CARTESIAN_POINT('Ctrl Pts',(207.38715854767,90.5272376084047,340.070293644044));
#23523=CARTESIAN_POINT('Ctrl Pts',(206.974311678662,90.4647376084047,341.870426808548));
#23524=CARTESIAN_POINT('Ctrl Pts',(205.409498490334,90.4022376084047,342.851386355541));
#23525=CARTESIAN_POINT('Ctrl Pts',(203.844685302007,90.3397376084047,343.832345902533));
#23526=CARTESIAN_POINT('Ctrl Pts',(202.044552137503,90.2772376084047,343.419499033524));
#23527=CARTESIAN_POINT('Ctrl Pts',(202.044552137503,91.0272376084047,343.419499033524));
#23528=CARTESIAN_POINT('Ctrl Pts',(200.244418972999,90.9647376084047,343.006652164516));
#23529=CARTESIAN_POINT('Ctrl Pts',(199.263459426007,90.9022376084047,341.441838976189));
#23530=CARTESIAN_POINT('Ctrl Pts',(198.282499879015,90.8397376084047,339.877025787862));
#23531=CARTESIAN_POINT('Ctrl Pts',(198.695346748023,90.7772376084047,338.076892623358));
#23532=CARTESIAN_POINT('Ctrl Pts',(199.108193617031,90.7147376084047,336.276759458854));
#23533=CARTESIAN_POINT('Ctrl Pts',(200.673006805358,90.6522376084047,335.295799911861));
#23534=CARTESIAN_POINT('Ctrl Pts',(202.237819993686,90.5897376084047,334.314840364869));
#23535=CARTESIAN_POINT('Ctrl Pts',(204.03795315819,90.5272376084047,334.727687233877));
#23536=CARTESIAN_POINT('Ctrl Pts',(205.838086322694,90.4647376084047,335.140534102886));
#23537=CARTESIAN_POINT('Ctrl Pts',(206.819045869686,90.4022376084047,336.705347291213));
#23538=CARTESIAN_POINT('Ctrl Pts',(207.800005416678,90.3397376084047,338.27016047954));
#23539=CARTESIAN_POINT('Ctrl Pts',(207.38715854767,90.2772376084047,340.070293644044));
#23540=CARTESIAN_POINT('Ctrl Pts',(206.974311678662,90.2147376084047,341.870426808548));
#23541=CARTESIAN_POINT('Ctrl Pts',(205.409498490334,90.1522376084047,342.851386355541));
#23542=CARTESIAN_POINT('Ctrl Pts',(203.844685302007,90.0897376084047,343.832345902533));
#23543=CARTESIAN_POINT('Ctrl Pts',(202.044552137503,90.0272376084047,343.419499033524));
#23544=CARTESIAN_POINT('Origin',(203.041252647847,101.652237608405,339.0735931337));
#23545=CARTESIAN_POINT('',(202.044552137503,92.2772376084047,343.419499033524));
#23546=CARTESIAN_POINT('',(202.044552137503,92.0272376084047,343.419499033524));
#23547=CARTESIAN_POINT('',(202.044552137504,101.652237608405,343.419499033523));
#23548=CARTESIAN_POINT('Ctrl Pts',(202.044552137503,92.2772376084047,343.419499033524));
#23549=CARTESIAN_POINT('Ctrl Pts',(200.244418972999,92.2147376084047,343.006652164516));
#23550=CARTESIAN_POINT('Ctrl Pts',(199.263459426007,92.1522376084047,341.441838976189));
#23551=CARTESIAN_POINT('Ctrl Pts',(198.282499879015,92.0897376084047,339.877025787862));
#23552=CARTESIAN_POINT('Ctrl Pts',(198.695346748023,92.0272376084047,338.076892623358));
#23553=CARTESIAN_POINT('Ctrl Pts',(199.108193617031,91.9647376084047,336.276759458854));
#23554=CARTESIAN_POINT('Ctrl Pts',(200.673006805358,91.9022376084047,335.295799911861));
#23555=CARTESIAN_POINT('Ctrl Pts',(202.237819993686,91.8397376084047,334.314840364869));
#23556=CARTESIAN_POINT('Ctrl Pts',(204.03795315819,91.7772376084047,334.727687233877));
#23557=CARTESIAN_POINT('Ctrl Pts',(205.838086322694,91.7147376084047,335.140534102886));
#23558=CARTESIAN_POINT('Ctrl Pts',(206.819045869686,91.6522376084047,336.705347291213));
#23559=CARTESIAN_POINT('Ctrl Pts',(207.800005416678,91.5897376084047,338.27016047954));
#23560=CARTESIAN_POINT('Ctrl Pts',(207.38715854767,91.5272376084047,340.070293644044));
#23561=CARTESIAN_POINT('Ctrl Pts',(206.974311678662,91.4647376084047,341.870426808548));
#23562=CARTESIAN_POINT('Ctrl Pts',(205.409498490334,91.4022376084047,342.851386355541));
#23563=CARTESIAN_POINT('Ctrl Pts',(203.844685302007,91.3397376084047,343.832345902533));
#23564=CARTESIAN_POINT('Ctrl Pts',(202.044552137503,91.2772376084047,343.419499033524));
#23565=CARTESIAN_POINT('Ctrl Pts',(202.044552137503,92.0272376084047,343.419499033524));
#23566=CARTESIAN_POINT('Ctrl Pts',(200.244418972999,91.9647376084047,343.006652164516));
#23567=CARTESIAN_POINT('Ctrl Pts',(199.263459426007,91.9022376084047,341.441838976189));
#23568=CARTESIAN_POINT('Ctrl Pts',(198.282499879015,91.8397376084047,339.877025787862));
#23569=CARTESIAN_POINT('Ctrl Pts',(198.695346748023,91.7772376084047,338.076892623358));
#23570=CARTESIAN_POINT('Ctrl Pts',(199.108193617031,91.7147376084047,336.276759458854));
#23571=CARTESIAN_POINT('Ctrl Pts',(200.673006805358,91.6522376084047,335.295799911861));
#23572=CARTESIAN_POINT('Ctrl Pts',(202.237819993686,91.5897376084047,334.314840364869));
#23573=CARTESIAN_POINT('Ctrl Pts',(204.03795315819,91.5272376084047,334.727687233877));
#23574=CARTESIAN_POINT('Ctrl Pts',(205.838086322694,91.4647376084047,335.140534102886));
#23575=CARTESIAN_POINT('Ctrl Pts',(206.819045869686,91.4022376084047,336.705347291213));
#23576=CARTESIAN_POINT('Ctrl Pts',(207.800005416678,91.3397376084047,338.27016047954));
#23577=CARTESIAN_POINT('Ctrl Pts',(207.38715854767,91.2772376084047,340.070293644044));
#23578=CARTESIAN_POINT('Ctrl Pts',(206.974311678662,91.2147376084047,341.870426808548));
#23579=CARTESIAN_POINT('Ctrl Pts',(205.409498490334,91.1522376084047,342.851386355541));
#23580=CARTESIAN_POINT('Ctrl Pts',(203.844685302007,91.0897376084047,343.832345902533));
#23581=CARTESIAN_POINT('Ctrl Pts',(202.044552137503,91.0272376084047,343.419499033524));
#23582=CARTESIAN_POINT('Origin',(203.041252647847,101.652237608405,339.0735931337));
#23583=CARTESIAN_POINT('',(202.044552137503,93.2772376084047,343.419499033524));
#23584=CARTESIAN_POINT('',(202.044552137503,93.0272376084047,343.419499033524));
#23585=CARTESIAN_POINT('',(202.044552137504,101.652237608405,343.419499033523));
#23586=CARTESIAN_POINT('Ctrl Pts',(202.044552137503,93.2772376084047,343.419499033524));
#23587=CARTESIAN_POINT('Ctrl Pts',(200.244418972999,93.2147376084047,343.006652164516));
#23588=CARTESIAN_POINT('Ctrl Pts',(199.263459426007,93.1522376084047,341.441838976189));
#23589=CARTESIAN_POINT('Ctrl Pts',(198.282499879015,93.0897376084047,339.877025787862));
#23590=CARTESIAN_POINT('Ctrl Pts',(198.695346748023,93.0272376084047,338.076892623358));
#23591=CARTESIAN_POINT('Ctrl Pts',(199.108193617031,92.9647376084047,336.276759458854));
#23592=CARTESIAN_POINT('Ctrl Pts',(200.673006805358,92.9022376084047,335.295799911861));
#23593=CARTESIAN_POINT('Ctrl Pts',(202.237819993686,92.8397376084047,334.314840364869));
#23594=CARTESIAN_POINT('Ctrl Pts',(204.03795315819,92.7772376084047,334.727687233877));
#23595=CARTESIAN_POINT('Ctrl Pts',(205.838086322694,92.7147376084047,335.140534102886));
#23596=CARTESIAN_POINT('Ctrl Pts',(206.819045869686,92.6522376084047,336.705347291213));
#23597=CARTESIAN_POINT('Ctrl Pts',(207.800005416678,92.5897376084047,338.27016047954));
#23598=CARTESIAN_POINT('Ctrl Pts',(207.38715854767,92.5272376084047,340.070293644044));
#23599=CARTESIAN_POINT('Ctrl Pts',(206.974311678662,92.4647376084047,341.870426808548));
#23600=CARTESIAN_POINT('Ctrl Pts',(205.409498490334,92.4022376084047,342.851386355541));
#23601=CARTESIAN_POINT('Ctrl Pts',(203.844685302007,92.3397376084047,343.832345902533));
#23602=CARTESIAN_POINT('Ctrl Pts',(202.044552137503,92.2772376084047,343.419499033524));
#23603=CARTESIAN_POINT('Ctrl Pts',(202.044552137503,93.0272376084047,343.419499033524));
#23604=CARTESIAN_POINT('Ctrl Pts',(200.244418972999,92.9647376084047,343.006652164516));
#23605=CARTESIAN_POINT('Ctrl Pts',(199.263459426007,92.9022376084047,341.441838976189));
#23606=CARTESIAN_POINT('Ctrl Pts',(198.282499879015,92.8397376084047,339.877025787862));
#23607=CARTESIAN_POINT('Ctrl Pts',(198.695346748023,92.7772376084047,338.076892623358));
#23608=CARTESIAN_POINT('Ctrl Pts',(199.108193617031,92.7147376084047,336.276759458854));
#23609=CARTESIAN_POINT('Ctrl Pts',(200.673006805358,92.6522376084047,335.295799911861));
#23610=CARTESIAN_POINT('Ctrl Pts',(202.237819993686,92.5897376084047,334.314840364869));
#23611=CARTESIAN_POINT('Ctrl Pts',(204.03795315819,92.5272376084047,334.727687233877));
#23612=CARTESIAN_POINT('Ctrl Pts',(205.838086322694,92.4647376084047,335.140534102886));
#23613=CARTESIAN_POINT('Ctrl Pts',(206.819045869686,92.4022376084047,336.705347291213));
#23614=CARTESIAN_POINT('Ctrl Pts',(207.800005416678,92.3397376084047,338.27016047954));
#23615=CARTESIAN_POINT('Ctrl Pts',(207.38715854767,92.2772376084047,340.070293644044));
#23616=CARTESIAN_POINT('Ctrl Pts',(206.974311678662,92.2147376084047,341.870426808548));
#23617=CARTESIAN_POINT('Ctrl Pts',(205.409498490334,92.1522376084047,342.851386355541));
#23618=CARTESIAN_POINT('Ctrl Pts',(203.844685302007,92.0897376084047,343.832345902533));
#23619=CARTESIAN_POINT('Ctrl Pts',(202.044552137503,92.0272376084047,343.419499033524));
#23620=CARTESIAN_POINT('Origin',(203.041252647847,101.652237608405,339.0735931337));
#23621=CARTESIAN_POINT('',(202.044552137503,94.2772376084047,343.419499033524));
#23622=CARTESIAN_POINT('',(202.044552137503,94.0272376084047,343.419499033524));
#23623=CARTESIAN_POINT('',(202.044552137504,101.652237608405,343.419499033523));
#23624=CARTESIAN_POINT('Ctrl Pts',(202.044552137503,94.2772376084047,343.419499033524));
#23625=CARTESIAN_POINT('Ctrl Pts',(200.244418972999,94.2147376084047,343.006652164516));
#23626=CARTESIAN_POINT('Ctrl Pts',(199.263459426007,94.1522376084047,341.441838976189));
#23627=CARTESIAN_POINT('Ctrl Pts',(198.282499879015,94.0897376084047,339.877025787862));
#23628=CARTESIAN_POINT('Ctrl Pts',(198.695346748023,94.0272376084047,338.076892623358));
#23629=CARTESIAN_POINT('Ctrl Pts',(199.108193617031,93.9647376084047,336.276759458854));
#23630=CARTESIAN_POINT('Ctrl Pts',(200.673006805358,93.9022376084047,335.295799911861));
#23631=CARTESIAN_POINT('Ctrl Pts',(202.237819993686,93.8397376084047,334.314840364869));
#23632=CARTESIAN_POINT('Ctrl Pts',(204.03795315819,93.7772376084047,334.727687233877));
#23633=CARTESIAN_POINT('Ctrl Pts',(205.838086322694,93.7147376084047,335.140534102886));
#23634=CARTESIAN_POINT('Ctrl Pts',(206.819045869686,93.6522376084047,336.705347291213));
#23635=CARTESIAN_POINT('Ctrl Pts',(207.800005416678,93.5897376084047,338.27016047954));
#23636=CARTESIAN_POINT('Ctrl Pts',(207.38715854767,93.5272376084047,340.070293644044));
#23637=CARTESIAN_POINT('Ctrl Pts',(206.974311678662,93.4647376084047,341.870426808548));
#23638=CARTESIAN_POINT('Ctrl Pts',(205.409498490334,93.4022376084047,342.851386355541));
#23639=CARTESIAN_POINT('Ctrl Pts',(203.844685302007,93.3397376084047,343.832345902533));
#23640=CARTESIAN_POINT('Ctrl Pts',(202.044552137503,93.2772376084047,343.419499033524));
#23641=CARTESIAN_POINT('Ctrl Pts',(202.044552137503,94.0272376084047,343.419499033524));
#23642=CARTESIAN_POINT('Ctrl Pts',(200.244418972999,93.9647376084047,343.006652164516));
#23643=CARTESIAN_POINT('Ctrl Pts',(199.263459426007,93.9022376084047,341.441838976189));
#23644=CARTESIAN_POINT('Ctrl Pts',(198.282499879015,93.8397376084047,339.877025787862));
#23645=CARTESIAN_POINT('Ctrl Pts',(198.695346748023,93.7772376084047,338.076892623358));
#23646=CARTESIAN_POINT('Ctrl Pts',(199.108193617031,93.7147376084047,336.276759458854));
#23647=CARTESIAN_POINT('Ctrl Pts',(200.673006805358,93.6522376084047,335.295799911861));
#23648=CARTESIAN_POINT('Ctrl Pts',(202.237819993686,93.5897376084047,334.314840364869));
#23649=CARTESIAN_POINT('Ctrl Pts',(204.03795315819,93.5272376084047,334.727687233877));
#23650=CARTESIAN_POINT('Ctrl Pts',(205.838086322694,93.4647376084047,335.140534102886));
#23651=CARTESIAN_POINT('Ctrl Pts',(206.819045869686,93.4022376084047,336.705347291213));
#23652=CARTESIAN_POINT('Ctrl Pts',(207.800005416678,93.3397376084047,338.27016047954));
#23653=CARTESIAN_POINT('Ctrl Pts',(207.38715854767,93.2772376084047,340.070293644044));
#23654=CARTESIAN_POINT('Ctrl Pts',(206.974311678662,93.2147376084047,341.870426808548));
#23655=CARTESIAN_POINT('Ctrl Pts',(205.409498490334,93.1522376084047,342.851386355541));
#23656=CARTESIAN_POINT('Ctrl Pts',(203.844685302007,93.0897376084047,343.832345902533));
#23657=CARTESIAN_POINT('Ctrl Pts',(202.044552137503,93.0272376084047,343.419499033524));
#23658=CARTESIAN_POINT('Origin',(203.041252647847,101.652237608405,339.0735931337));
#23659=CARTESIAN_POINT('',(202.044552137503,95.2772376084047,343.419499033524));
#23660=CARTESIAN_POINT('',(202.044552137503,95.0272376084047,343.419499033524));
#23661=CARTESIAN_POINT('',(202.044552137504,101.652237608405,343.419499033523));
#23662=CARTESIAN_POINT('Ctrl Pts',(202.044552137503,95.2772376084047,343.419499033524));
#23663=CARTESIAN_POINT('Ctrl Pts',(200.244418972999,95.2147376084047,343.006652164516));
#23664=CARTESIAN_POINT('Ctrl Pts',(199.263459426007,95.1522376084047,341.441838976189));
#23665=CARTESIAN_POINT('Ctrl Pts',(198.282499879015,95.0897376084047,339.877025787862));
#23666=CARTESIAN_POINT('Ctrl Pts',(198.695346748023,95.0272376084047,338.076892623358));
#23667=CARTESIAN_POINT('Ctrl Pts',(199.108193617031,94.9647376084047,336.276759458854));
#23668=CARTESIAN_POINT('Ctrl Pts',(200.673006805358,94.9022376084047,335.295799911861));
#23669=CARTESIAN_POINT('Ctrl Pts',(202.237819993686,94.8397376084047,334.314840364869));
#23670=CARTESIAN_POINT('Ctrl Pts',(204.03795315819,94.7772376084047,334.727687233877));
#23671=CARTESIAN_POINT('Ctrl Pts',(205.838086322694,94.7147376084047,335.140534102886));
#23672=CARTESIAN_POINT('Ctrl Pts',(206.819045869686,94.6522376084047,336.705347291213));
#23673=CARTESIAN_POINT('Ctrl Pts',(207.800005416678,94.5897376084047,338.27016047954));
#23674=CARTESIAN_POINT('Ctrl Pts',(207.38715854767,94.5272376084047,340.070293644044));
#23675=CARTESIAN_POINT('Ctrl Pts',(206.974311678662,94.4647376084047,341.870426808548));
#23676=CARTESIAN_POINT('Ctrl Pts',(205.409498490334,94.4022376084047,342.851386355541));
#23677=CARTESIAN_POINT('Ctrl Pts',(203.844685302007,94.3397376084047,343.832345902533));
#23678=CARTESIAN_POINT('Ctrl Pts',(202.044552137503,94.2772376084047,343.419499033524));
#23679=CARTESIAN_POINT('Ctrl Pts',(202.044552137503,95.0272376084047,343.419499033524));
#23680=CARTESIAN_POINT('Ctrl Pts',(200.244418972999,94.9647376084047,343.006652164516));
#23681=CARTESIAN_POINT('Ctrl Pts',(199.263459426007,94.9022376084047,341.441838976189));
#23682=CARTESIAN_POINT('Ctrl Pts',(198.282499879015,94.8397376084047,339.877025787862));
#23683=CARTESIAN_POINT('Ctrl Pts',(198.695346748023,94.7772376084047,338.076892623358));
#23684=CARTESIAN_POINT('Ctrl Pts',(199.108193617031,94.7147376084047,336.276759458854));
#23685=CARTESIAN_POINT('Ctrl Pts',(200.673006805358,94.6522376084047,335.295799911861));
#23686=CARTESIAN_POINT('Ctrl Pts',(202.237819993686,94.5897376084047,334.314840364869));
#23687=CARTESIAN_POINT('Ctrl Pts',(204.03795315819,94.5272376084047,334.727687233877));
#23688=CARTESIAN_POINT('Ctrl Pts',(205.838086322694,94.4647376084047,335.140534102886));
#23689=CARTESIAN_POINT('Ctrl Pts',(206.819045869686,94.4022376084047,336.705347291213));
#23690=CARTESIAN_POINT('Ctrl Pts',(207.800005416678,94.3397376084047,338.27016047954));
#23691=CARTESIAN_POINT('Ctrl Pts',(207.38715854767,94.2772376084047,340.070293644044));
#23692=CARTESIAN_POINT('Ctrl Pts',(206.974311678662,94.2147376084047,341.870426808548));
#23693=CARTESIAN_POINT('Ctrl Pts',(205.409498490334,94.1522376084047,342.851386355541));
#23694=CARTESIAN_POINT('Ctrl Pts',(203.844685302007,94.0897376084047,343.832345902533));
#23695=CARTESIAN_POINT('Ctrl Pts',(202.044552137503,94.0272376084047,343.419499033524));
#23696=CARTESIAN_POINT('Origin',(203.041252647847,101.652237608405,339.0735931337));
#23697=CARTESIAN_POINT('',(202.044552137503,96.2772376084047,343.419499033524));
#23698=CARTESIAN_POINT('',(202.044552137503,96.0272376084047,343.419499033524));
#23699=CARTESIAN_POINT('',(202.044552137504,101.652237608405,343.419499033523));
#23700=CARTESIAN_POINT('Ctrl Pts',(202.044552137503,96.2772376084047,343.419499033524));
#23701=CARTESIAN_POINT('Ctrl Pts',(200.244418972999,96.2147376084047,343.006652164516));
#23702=CARTESIAN_POINT('Ctrl Pts',(199.263459426007,96.1522376084047,341.441838976189));
#23703=CARTESIAN_POINT('Ctrl Pts',(198.282499879015,96.0897376084047,339.877025787862));
#23704=CARTESIAN_POINT('Ctrl Pts',(198.695346748023,96.0272376084047,338.076892623358));
#23705=CARTESIAN_POINT('Ctrl Pts',(199.108193617031,95.9647376084047,336.276759458854));
#23706=CARTESIAN_POINT('Ctrl Pts',(200.673006805358,95.9022376084047,335.295799911861));
#23707=CARTESIAN_POINT('Ctrl Pts',(202.237819993686,95.8397376084047,334.314840364869));
#23708=CARTESIAN_POINT('Ctrl Pts',(204.03795315819,95.7772376084047,334.727687233877));
#23709=CARTESIAN_POINT('Ctrl Pts',(205.838086322694,95.7147376084047,335.140534102886));
#23710=CARTESIAN_POINT('Ctrl Pts',(206.819045869686,95.6522376084047,336.705347291213));
#23711=CARTESIAN_POINT('Ctrl Pts',(207.800005416678,95.5897376084047,338.27016047954));
#23712=CARTESIAN_POINT('Ctrl Pts',(207.38715854767,95.5272376084047,340.070293644044));
#23713=CARTESIAN_POINT('Ctrl Pts',(206.974311678662,95.4647376084047,341.870426808548));
#23714=CARTESIAN_POINT('Ctrl Pts',(205.409498490334,95.4022376084047,342.851386355541));
#23715=CARTESIAN_POINT('Ctrl Pts',(203.844685302007,95.3397376084047,343.832345902533));
#23716=CARTESIAN_POINT('Ctrl Pts',(202.044552137503,95.2772376084047,343.419499033524));
#23717=CARTESIAN_POINT('Ctrl Pts',(202.044552137503,96.0272376084047,343.419499033524));
#23718=CARTESIAN_POINT('Ctrl Pts',(200.244418972999,95.9647376084047,343.006652164516));
#23719=CARTESIAN_POINT('Ctrl Pts',(199.263459426007,95.9022376084047,341.441838976189));
#23720=CARTESIAN_POINT('Ctrl Pts',(198.282499879015,95.8397376084047,339.877025787862));
#23721=CARTESIAN_POINT('Ctrl Pts',(198.695346748023,95.7772376084047,338.076892623358));
#23722=CARTESIAN_POINT('Ctrl Pts',(199.108193617031,95.7147376084047,336.276759458854));
#23723=CARTESIAN_POINT('Ctrl Pts',(200.673006805358,95.6522376084047,335.295799911861));
#23724=CARTESIAN_POINT('Ctrl Pts',(202.237819993686,95.5897376084047,334.314840364869));
#23725=CARTESIAN_POINT('Ctrl Pts',(204.03795315819,95.5272376084047,334.727687233877));
#23726=CARTESIAN_POINT('Ctrl Pts',(205.838086322694,95.4647376084047,335.140534102886));
#23727=CARTESIAN_POINT('Ctrl Pts',(206.819045869686,95.4022376084047,336.705347291213));
#23728=CARTESIAN_POINT('Ctrl Pts',(207.800005416678,95.3397376084047,338.27016047954));
#23729=CARTESIAN_POINT('Ctrl Pts',(207.38715854767,95.2772376084047,340.070293644044));
#23730=CARTESIAN_POINT('Ctrl Pts',(206.974311678662,95.2147376084047,341.870426808548));
#23731=CARTESIAN_POINT('Ctrl Pts',(205.409498490334,95.1522376084047,342.851386355541));
#23732=CARTESIAN_POINT('Ctrl Pts',(203.844685302007,95.0897376084047,343.832345902533));
#23733=CARTESIAN_POINT('Ctrl Pts',(202.044552137503,95.0272376084047,343.419499033524));
#23734=CARTESIAN_POINT('Origin',(203.041252647847,101.652237608405,339.0735931337));
#23735=CARTESIAN_POINT('',(202.044552137503,97.2772376084047,343.419499033524));
#23736=CARTESIAN_POINT('',(202.044552137503,97.0272376084047,343.419499033524));
#23737=CARTESIAN_POINT('',(202.044552137504,101.652237608405,343.419499033523));
#23738=CARTESIAN_POINT('Ctrl Pts',(202.044552137503,97.2772376084047,343.419499033524));
#23739=CARTESIAN_POINT('Ctrl Pts',(200.244418972999,97.2147376084047,343.006652164516));
#23740=CARTESIAN_POINT('Ctrl Pts',(199.263459426007,97.1522376084047,341.441838976189));
#23741=CARTESIAN_POINT('Ctrl Pts',(198.282499879015,97.0897376084047,339.877025787862));
#23742=CARTESIAN_POINT('Ctrl Pts',(198.695346748023,97.0272376084047,338.076892623358));
#23743=CARTESIAN_POINT('Ctrl Pts',(199.108193617031,96.9647376084047,336.276759458854));
#23744=CARTESIAN_POINT('Ctrl Pts',(200.673006805358,96.9022376084047,335.295799911861));
#23745=CARTESIAN_POINT('Ctrl Pts',(202.237819993686,96.8397376084047,334.314840364869));
#23746=CARTESIAN_POINT('Ctrl Pts',(204.03795315819,96.7772376084047,334.727687233877));
#23747=CARTESIAN_POINT('Ctrl Pts',(205.838086322694,96.7147376084047,335.140534102886));
#23748=CARTESIAN_POINT('Ctrl Pts',(206.819045869686,96.6522376084047,336.705347291213));
#23749=CARTESIAN_POINT('Ctrl Pts',(207.800005416678,96.5897376084047,338.27016047954));
#23750=CARTESIAN_POINT('Ctrl Pts',(207.38715854767,96.5272376084047,340.070293644044));
#23751=CARTESIAN_POINT('Ctrl Pts',(206.974311678662,96.4647376084047,341.870426808548));
#23752=CARTESIAN_POINT('Ctrl Pts',(205.409498490334,96.4022376084047,342.851386355541));
#23753=CARTESIAN_POINT('Ctrl Pts',(203.844685302007,96.3397376084047,343.832345902533));
#23754=CARTESIAN_POINT('Ctrl Pts',(202.044552137503,96.2772376084047,343.419499033524));
#23755=CARTESIAN_POINT('Ctrl Pts',(202.044552137503,97.0272376084047,343.419499033524));
#23756=CARTESIAN_POINT('Ctrl Pts',(200.244418972999,96.9647376084047,343.006652164516));
#23757=CARTESIAN_POINT('Ctrl Pts',(199.263459426007,96.9022376084047,341.441838976189));
#23758=CARTESIAN_POINT('Ctrl Pts',(198.282499879015,96.8397376084047,339.877025787862));
#23759=CARTESIAN_POINT('Ctrl Pts',(198.695346748023,96.7772376084047,338.076892623358));
#23760=CARTESIAN_POINT('Ctrl Pts',(199.108193617031,96.7147376084047,336.276759458854));
#23761=CARTESIAN_POINT('Ctrl Pts',(200.673006805358,96.6522376084047,335.295799911861));
#23762=CARTESIAN_POINT('Ctrl Pts',(202.237819993686,96.5897376084047,334.314840364869));
#23763=CARTESIAN_POINT('Ctrl Pts',(204.03795315819,96.5272376084047,334.727687233877));
#23764=CARTESIAN_POINT('Ctrl Pts',(205.838086322694,96.4647376084047,335.140534102886));
#23765=CARTESIAN_POINT('Ctrl Pts',(206.819045869686,96.4022376084047,336.705347291213));
#23766=CARTESIAN_POINT('Ctrl Pts',(207.800005416678,96.3397376084047,338.27016047954));
#23767=CARTESIAN_POINT('Ctrl Pts',(207.38715854767,96.2772376084047,340.070293644044));
#23768=CARTESIAN_POINT('Ctrl Pts',(206.974311678662,96.2147376084047,341.870426808548));
#23769=CARTESIAN_POINT('Ctrl Pts',(205.409498490334,96.1522376084047,342.851386355541));
#23770=CARTESIAN_POINT('Ctrl Pts',(203.844685302007,96.0897376084047,343.832345902533));
#23771=CARTESIAN_POINT('Ctrl Pts',(202.044552137503,96.0272376084047,343.419499033524));
#23772=CARTESIAN_POINT('Origin',(203.041252647847,101.652237608405,339.0735931337));
#23773=CARTESIAN_POINT('',(202.044552137503,98.2772376084047,343.419499033524));
#23774=CARTESIAN_POINT('',(202.044552137503,98.0272376084047,343.419499033524));
#23775=CARTESIAN_POINT('',(202.044552137504,101.652237608405,343.419499033523));
#23776=CARTESIAN_POINT('Ctrl Pts',(202.044552137503,98.2772376084047,343.419499033524));
#23777=CARTESIAN_POINT('Ctrl Pts',(200.244418972999,98.2147376084047,343.006652164516));
#23778=CARTESIAN_POINT('Ctrl Pts',(199.263459426007,98.1522376084047,341.441838976189));
#23779=CARTESIAN_POINT('Ctrl Pts',(198.282499879015,98.0897376084047,339.877025787862));
#23780=CARTESIAN_POINT('Ctrl Pts',(198.695346748023,98.0272376084047,338.076892623358));
#23781=CARTESIAN_POINT('Ctrl Pts',(199.108193617031,97.9647376084047,336.276759458854));
#23782=CARTESIAN_POINT('Ctrl Pts',(200.673006805358,97.9022376084047,335.295799911861));
#23783=CARTESIAN_POINT('Ctrl Pts',(202.237819993686,97.8397376084047,334.314840364869));
#23784=CARTESIAN_POINT('Ctrl Pts',(204.03795315819,97.7772376084047,334.727687233877));
#23785=CARTESIAN_POINT('Ctrl Pts',(205.838086322694,97.7147376084047,335.140534102886));
#23786=CARTESIAN_POINT('Ctrl Pts',(206.819045869686,97.6522376084047,336.705347291213));
#23787=CARTESIAN_POINT('Ctrl Pts',(207.800005416678,97.5897376084047,338.27016047954));
#23788=CARTESIAN_POINT('Ctrl Pts',(207.38715854767,97.5272376084047,340.070293644044));
#23789=CARTESIAN_POINT('Ctrl Pts',(206.974311678662,97.4647376084047,341.870426808548));
#23790=CARTESIAN_POINT('Ctrl Pts',(205.409498490334,97.4022376084047,342.851386355541));
#23791=CARTESIAN_POINT('Ctrl Pts',(203.844685302007,97.3397376084047,343.832345902533));
#23792=CARTESIAN_POINT('Ctrl Pts',(202.044552137503,97.2772376084047,343.419499033524));
#23793=CARTESIAN_POINT('Ctrl Pts',(202.044552137503,98.0272376084047,343.419499033524));
#23794=CARTESIAN_POINT('Ctrl Pts',(200.244418972999,97.9647376084047,343.006652164516));
#23795=CARTESIAN_POINT('Ctrl Pts',(199.263459426007,97.9022376084047,341.441838976189));
#23796=CARTESIAN_POINT('Ctrl Pts',(198.282499879015,97.8397376084047,339.877025787862));
#23797=CARTESIAN_POINT('Ctrl Pts',(198.695346748023,97.7772376084047,338.076892623358));
#23798=CARTESIAN_POINT('Ctrl Pts',(199.108193617031,97.7147376084047,336.276759458854));
#23799=CARTESIAN_POINT('Ctrl Pts',(200.673006805358,97.6522376084047,335.295799911861));
#23800=CARTESIAN_POINT('Ctrl Pts',(202.237819993686,97.5897376084047,334.314840364869));
#23801=CARTESIAN_POINT('Ctrl Pts',(204.03795315819,97.5272376084047,334.727687233877));
#23802=CARTESIAN_POINT('Ctrl Pts',(205.838086322694,97.4647376084047,335.140534102886));
#23803=CARTESIAN_POINT('Ctrl Pts',(206.819045869686,97.4022376084047,336.705347291213));
#23804=CARTESIAN_POINT('Ctrl Pts',(207.800005416678,97.3397376084047,338.27016047954));
#23805=CARTESIAN_POINT('Ctrl Pts',(207.38715854767,97.2772376084047,340.070293644044));
#23806=CARTESIAN_POINT('Ctrl Pts',(206.974311678662,97.2147376084047,341.870426808548));
#23807=CARTESIAN_POINT('Ctrl Pts',(205.409498490334,97.1522376084047,342.851386355541));
#23808=CARTESIAN_POINT('Ctrl Pts',(203.844685302007,97.0897376084047,343.832345902533));
#23809=CARTESIAN_POINT('Ctrl Pts',(202.044552137503,97.0272376084047,343.419499033524));
#23810=CARTESIAN_POINT('Origin',(203.041252647847,101.652237608405,339.0735931337));
#23811=CARTESIAN_POINT('',(202.044552137503,99.2772376084047,343.419499033524));
#23812=CARTESIAN_POINT('',(202.044552137503,99.0272376084047,343.419499033524));
#23813=CARTESIAN_POINT('',(202.044552137504,101.652237608405,343.419499033523));
#23814=CARTESIAN_POINT('Ctrl Pts',(202.044552137503,99.2772376084047,343.419499033524));
#23815=CARTESIAN_POINT('Ctrl Pts',(200.244418972999,99.2147376084047,343.006652164516));
#23816=CARTESIAN_POINT('Ctrl Pts',(199.263459426007,99.1522376084047,341.441838976189));
#23817=CARTESIAN_POINT('Ctrl Pts',(198.282499879015,99.0897376084047,339.877025787862));
#23818=CARTESIAN_POINT('Ctrl Pts',(198.695346748023,99.0272376084047,338.076892623358));
#23819=CARTESIAN_POINT('Ctrl Pts',(199.108193617031,98.9647376084047,336.276759458854));
#23820=CARTESIAN_POINT('Ctrl Pts',(200.673006805358,98.9022376084047,335.295799911861));
#23821=CARTESIAN_POINT('Ctrl Pts',(202.237819993686,98.8397376084047,334.314840364869));
#23822=CARTESIAN_POINT('Ctrl Pts',(204.03795315819,98.7772376084047,334.727687233877));
#23823=CARTESIAN_POINT('Ctrl Pts',(205.838086322694,98.7147376084047,335.140534102886));
#23824=CARTESIAN_POINT('Ctrl Pts',(206.819045869686,98.6522376084047,336.705347291213));
#23825=CARTESIAN_POINT('Ctrl Pts',(207.800005416678,98.5897376084047,338.27016047954));
#23826=CARTESIAN_POINT('Ctrl Pts',(207.38715854767,98.5272376084047,340.070293644044));
#23827=CARTESIAN_POINT('Ctrl Pts',(206.974311678662,98.4647376084047,341.870426808548));
#23828=CARTESIAN_POINT('Ctrl Pts',(205.409498490334,98.4022376084047,342.851386355541));
#23829=CARTESIAN_POINT('Ctrl Pts',(203.844685302007,98.3397376084047,343.832345902533));
#23830=CARTESIAN_POINT('Ctrl Pts',(202.044552137503,98.2772376084047,343.419499033524));
#23831=CARTESIAN_POINT('Ctrl Pts',(202.044552137503,99.0272376084047,343.419499033524));
#23832=CARTESIAN_POINT('Ctrl Pts',(200.244418972999,98.9647376084047,343.006652164516));
#23833=CARTESIAN_POINT('Ctrl Pts',(199.263459426007,98.9022376084047,341.441838976189));
#23834=CARTESIAN_POINT('Ctrl Pts',(198.282499879015,98.8397376084047,339.877025787862));
#23835=CARTESIAN_POINT('Ctrl Pts',(198.695346748023,98.7772376084047,338.076892623358));
#23836=CARTESIAN_POINT('Ctrl Pts',(199.108193617031,98.7147376084047,336.276759458854));
#23837=CARTESIAN_POINT('Ctrl Pts',(200.673006805358,98.6522376084047,335.295799911861));
#23838=CARTESIAN_POINT('Ctrl Pts',(202.237819993686,98.5897376084047,334.314840364869));
#23839=CARTESIAN_POINT('Ctrl Pts',(204.03795315819,98.5272376084047,334.727687233877));
#23840=CARTESIAN_POINT('Ctrl Pts',(205.838086322694,98.4647376084047,335.140534102886));
#23841=CARTESIAN_POINT('Ctrl Pts',(206.819045869686,98.4022376084047,336.705347291213));
#23842=CARTESIAN_POINT('Ctrl Pts',(207.800005416678,98.3397376084047,338.27016047954));
#23843=CARTESIAN_POINT('Ctrl Pts',(207.38715854767,98.2772376084047,340.070293644044));
#23844=CARTESIAN_POINT('Ctrl Pts',(206.974311678662,98.2147376084047,341.870426808548));
#23845=CARTESIAN_POINT('Ctrl Pts',(205.409498490334,98.1522376084047,342.851386355541));
#23846=CARTESIAN_POINT('Ctrl Pts',(203.844685302007,98.0897376084047,343.832345902533));
#23847=CARTESIAN_POINT('Ctrl Pts',(202.044552137503,98.0272376084047,343.419499033524));
#23848=CARTESIAN_POINT('Origin',(203.041252647847,101.652237608405,339.0735931337));
#23849=CARTESIAN_POINT('',(202.044552137503,100.277237608405,343.419499033524));
#23850=CARTESIAN_POINT('',(202.044552137503,100.027237608405,343.419499033524));
#23851=CARTESIAN_POINT('',(202.044552137504,101.652237608405,343.419499033523));
#23852=CARTESIAN_POINT('Ctrl Pts',(202.044552137503,100.277237608405,343.419499033524));
#23853=CARTESIAN_POINT('Ctrl Pts',(200.244418972999,100.214737608405,343.006652164516));
#23854=CARTESIAN_POINT('Ctrl Pts',(199.263459426007,100.152237608405,341.441838976189));
#23855=CARTESIAN_POINT('Ctrl Pts',(198.282499879015,100.089737608405,339.877025787862));
#23856=CARTESIAN_POINT('Ctrl Pts',(198.695346748023,100.027237608405,338.076892623358));
#23857=CARTESIAN_POINT('Ctrl Pts',(199.108193617031,99.9647376084047,336.276759458854));
#23858=CARTESIAN_POINT('Ctrl Pts',(200.673006805358,99.9022376084047,335.295799911861));
#23859=CARTESIAN_POINT('Ctrl Pts',(202.237819993686,99.8397376084047,334.314840364869));
#23860=CARTESIAN_POINT('Ctrl Pts',(204.03795315819,99.7772376084047,334.727687233877));
#23861=CARTESIAN_POINT('Ctrl Pts',(205.838086322694,99.7147376084047,335.140534102886));
#23862=CARTESIAN_POINT('Ctrl Pts',(206.819045869686,99.6522376084047,336.705347291213));
#23863=CARTESIAN_POINT('Ctrl Pts',(207.800005416678,99.5897376084047,338.27016047954));
#23864=CARTESIAN_POINT('Ctrl Pts',(207.38715854767,99.5272376084047,340.070293644044));
#23865=CARTESIAN_POINT('Ctrl Pts',(206.974311678662,99.4647376084047,341.870426808548));
#23866=CARTESIAN_POINT('Ctrl Pts',(205.409498490334,99.4022376084047,342.851386355541));
#23867=CARTESIAN_POINT('Ctrl Pts',(203.844685302007,99.3397376084047,343.832345902533));
#23868=CARTESIAN_POINT('Ctrl Pts',(202.044552137503,99.2772376084047,343.419499033524));
#23869=CARTESIAN_POINT('Ctrl Pts',(202.044552137503,100.027237608405,343.419499033524));
#23870=CARTESIAN_POINT('Ctrl Pts',(200.244418972999,99.9647376084047,343.006652164516));
#23871=CARTESIAN_POINT('Ctrl Pts',(199.263459426007,99.9022376084047,341.441838976189));
#23872=CARTESIAN_POINT('Ctrl Pts',(198.282499879015,99.8397376084047,339.877025787862));
#23873=CARTESIAN_POINT('Ctrl Pts',(198.695346748023,99.7772376084047,338.076892623358));
#23874=CARTESIAN_POINT('Ctrl Pts',(199.108193617031,99.7147376084047,336.276759458854));
#23875=CARTESIAN_POINT('Ctrl Pts',(200.673006805358,99.6522376084047,335.295799911861));
#23876=CARTESIAN_POINT('Ctrl Pts',(202.237819993686,99.5897376084047,334.314840364869));
#23877=CARTESIAN_POINT('Ctrl Pts',(204.03795315819,99.5272376084047,334.727687233877));
#23878=CARTESIAN_POINT('Ctrl Pts',(205.838086322694,99.4647376084047,335.140534102886));
#23879=CARTESIAN_POINT('Ctrl Pts',(206.819045869686,99.4022376084047,336.705347291213));
#23880=CARTESIAN_POINT('Ctrl Pts',(207.800005416678,99.3397376084047,338.27016047954));
#23881=CARTESIAN_POINT('Ctrl Pts',(207.38715854767,99.2772376084047,340.070293644044));
#23882=CARTESIAN_POINT('Ctrl Pts',(206.974311678662,99.2147376084047,341.870426808548));
#23883=CARTESIAN_POINT('Ctrl Pts',(205.409498490334,99.1522376084047,342.851386355541));
#23884=CARTESIAN_POINT('Ctrl Pts',(203.844685302007,99.0897376084047,343.832345902533));
#23885=CARTESIAN_POINT('Ctrl Pts',(202.044552137503,99.0272376084047,343.419499033524));
#23886=CARTESIAN_POINT('Origin',(203.041252647846,100.739737607039,339.073593133701));
#23887=CARTESIAN_POINT('',(207.914727694784,88.9647376097703,340.191287620971));
#23888=CARTESIAN_POINT('',(207.914727694784,88.8397376070391,340.191287620971));
#23889=CARTESIAN_POINT('',(207.914727694784,100.739737607039,340.191287620971));
#23890=CARTESIAN_POINT('',(207.914727694784,87.9647376097703,340.191287620971));
#23891=CARTESIAN_POINT('Ctrl Pts',(207.914727694784,88.9647376097703,340.191287620971));
#23892=CARTESIAN_POINT('Ctrl Pts',(207.770753734705,88.9453011777326,340.819056219497));
#23893=CARTESIAN_POINT('Ctrl Pts',(207.506770801709,88.9244834292568,341.413375945422));
#23894=CARTESIAN_POINT('Ctrl Pts',(206.767868521896,88.8824038680257,342.468698351296));
#23895=CARTESIAN_POINT('Ctrl Pts',(206.30024443967,88.8615432713098,342.919816661895));
#23896=CARTESIAN_POINT('Ctrl Pts',(205.201281739421,88.8217871525201,343.63181433124));
#23897=CARTESIAN_POINT('Ctrl Pts',(204.575887476526,88.8005368278284,343.878602026753));
#23898=CARTESIAN_POINT('Ctrl Pts',(203.286672824674,88.7577611328256,344.10890345328));
#23899=CARTESIAN_POINT('Ctrl Pts',(202.636859979253,88.7368875976579,344.098640860192));
#23900=CARTESIAN_POINT('Ctrl Pts',(201.355999128455,88.6971060741293,343.827800694488));
#23901=CARTESIAN_POINT('Ctrl Pts',(200.739055575249,88.6759104064177,343.561639678486));
#23902=CARTESIAN_POINT('Ctrl Pts',(199.663036126355,88.6331442992501,342.815574264922));
#23903=CARTESIAN_POINT('Ctrl Pts',(199.209615349934,88.6122569948317,342.349777136382));
#23904=CARTESIAN_POINT('Ctrl Pts',(198.493072284917,88.5724483372744,341.254430931273));
#23905=CARTESIAN_POINT('Ctrl Pts',(198.243690702334,88.5513105760968,340.630993961543));
#23906=CARTESIAN_POINT('Ctrl Pts',(198.007154195593,88.5085548963122,339.343453425775));
#23907=CARTESIAN_POINT('Ctrl Pts',(198.014285869939,88.4876529600333,338.693287385656));
#23908=CARTESIAN_POINT('Ctrl Pts',(198.278942152579,88.4478153546861,337.411729351262));
#23909=CARTESIAN_POINT('Ctrl Pts',(198.541659664048,88.4267388277125,336.794305791636));
#23910=CARTESIAN_POINT('Ctrl Pts',(199.281733177753,88.3839944866977,335.714843116983));
#23911=CARTESIAN_POINT('Ctrl Pts',(199.745420114066,88.3630770264696,335.258788929538));
#23912=CARTESIAN_POINT('Ctrl Pts',(200.836607730856,88.3232085762271,334.537042480549));
#23913=CARTESIAN_POINT('Ctrl Pts',(201.457803398381,88.3021966711763,334.284696586011));
#23914=CARTESIAN_POINT('Ctrl Pts',(202.743405108092,88.2594646574403,334.041028494398));
#23915=CARTESIAN_POINT('Ctrl Pts',(203.393957507691,88.2385307547311,334.044570031733));
#23916=CARTESIAN_POINT('Ctrl Pts',(204.676297004713,88.1986294812628,334.302146514328));
#23917=CARTESIAN_POINT('Ctrl Pts',(205.294264394291,88.1776856240901,334.560933524853));
#23918=CARTESIAN_POINT('Ctrl Pts',(206.37763782029,88.1349670086806,335.294148511304));
#23919=CARTESIAN_POINT('Ctrl Pts',(206.836690788396,88.1140157223278,335.755405346023));
#23920=CARTESIAN_POINT('Ctrl Pts',(207.564369000081,88.0740795693206,336.841827957796));
#23921=CARTESIAN_POINT('Ctrl Pts',(207.820087736203,88.0532071983605,337.460467803297));
#23922=CARTESIAN_POINT('Ctrl Pts',(208.071877720026,88.0105031403483,338.743830305215));
#23923=CARTESIAN_POINT('Ctrl Pts',(208.072436481244,87.9895335112199,339.394799672281));
#23924=CARTESIAN_POINT('Ctrl Pts',(207.938701912113,87.968107885949,340.082599871997));
#23925=CARTESIAN_POINT('Ctrl Pts',(207.927163070987,87.9664163810168,340.137065741634));
#23926=CARTESIAN_POINT('Ctrl Pts',(207.914727694784,87.9647376097703,340.191287620971));
#23927=CARTESIAN_POINT('',(207.914727694784,85.7397376070391,340.191287620971));
#23928=CARTESIAN_POINT('',(207.914727694784,100.739737607039,340.191287620971));
#23929=CARTESIAN_POINT('Origin',(203.041252647846,85.7397376070391,339.073593133701));
#23930=CARTESIAN_POINT('',(204.158947135117,87.2147376097703,334.200118086763));
#23931=CARTESIAN_POINT('Ctrl Pts',(207.914727694784,87.9647376097703,340.191287620971));
#23932=CARTESIAN_POINT('Ctrl Pts',(207.779340168193,87.946460343118,340.781616856755));
#23933=CARTESIAN_POINT('Ctrl Pts',(207.53769820905,87.9269437466332,341.342944322924));
#23934=CARTESIAN_POINT('Ctrl Pts',(206.843213031075,87.8860746366299,342.384380270813));
#23935=CARTESIAN_POINT('Ctrl Pts',(206.38474502582,87.8650856931962,342.846831028044));
#23936=CARTESIAN_POINT('Ctrl Pts',(205.303760064132,87.8250733241061,343.581239138041));
#23937=CARTESIAN_POINT('Ctrl Pts',(204.68802080038,87.8043541348048,343.840776520152));
#23938=CARTESIAN_POINT('Ctrl Pts',(203.407235979897,87.7616830481099,344.101770828163));
#23939=CARTESIAN_POINT('Ctrl Pts',(202.755823948159,87.74067381298,344.106991129162));
#23940=CARTESIAN_POINT('Ctrl Pts',(201.471656924595,87.7006199795155,343.866645597679));
#23941=CARTESIAN_POINT('Ctrl Pts',(200.852390116532,87.6799823415197,343.617372251638));
#23942=CARTESIAN_POINT('Ctrl Pts',(199.759636945518,87.6373298715157,342.900841860573));
#23943=CARTESIAN_POINT('Ctrl Pts',(199.293358206015,87.6162993689764,342.445561511859));
#23944=CARTESIAN_POINT('Ctrl Pts',(198.551355972455,87.5762017622807,341.370752937042));
#23945=CARTESIAN_POINT('Ctrl Pts',(198.287519423439,87.5556488164053,340.758287651802));
#23946=CARTESIAN_POINT('Ctrl Pts',(198.016152199308,87.5130165270529,339.480458695237));
#23947=CARTESIAN_POINT('Ctrl Pts',(198.005659980213,87.4919637916292,338.828586140853));
#23948=CARTESIAN_POINT('Ctrl Pts',(198.23566858912,87.451820062317,337.543373246385));
#23949=CARTESIAN_POINT('Ctrl Pts',(198.479269848345,87.4313547653813,336.923342329837));
#23950=CARTESIAN_POINT('Ctrl Pts',(199.185797327074,87.3887443333827,335.825055199215));
#23951=CARTESIAN_POINT('Ctrl Pts',(199.637451092009,87.3676684194138,335.354491635781));
#23952=CARTESIAN_POINT('Ctrl Pts',(200.705281337784,87.327476190036,334.6039724502));
#23953=CARTESIAN_POINT('Ctrl Pts',(201.314073893669,87.3071012622527,334.335326173143));
#23954=CARTESIAN_POINT('Ctrl Pts',(202.322427028207,87.2734064507242,334.111428557303));
#23955=CARTESIAN_POINT('Ctrl Pts',(202.695363361447,87.2611781225391,334.071578327997));
#23956=CARTESIAN_POINT('Ctrl Pts',(203.436005015253,87.2373458911319,334.075724784825));
#23957=CARTESIAN_POINT('Ctrl Pts',(203.801439960117,87.2258064397917,334.118126531495));
#23958=CARTESIAN_POINT('Ctrl Pts',(204.158947135117,87.2147376097703,334.200118086763));
#23959=CARTESIAN_POINT('',(204.158947135117,88.0897376070391,334.200118086763));
#23960=CARTESIAN_POINT('',(204.158947135117,87.6522376084047,334.200118086763));
#23961=CARTESIAN_POINT('Ctrl Pts',(204.158947135117,88.0897376070391,334.200118086763));
#23962=CARTESIAN_POINT('Ctrl Pts',(203.54376721609,88.108784279197,334.059031244714));
#23963=CARTESIAN_POINT('Ctrl Pts',(202.907424402043,88.1291528952381,334.035698514464));
#23964=CARTESIAN_POINT('Ctrl Pts',(201.658010954093,88.1704358529046,334.227232493023));
#23965=CARTESIAN_POINT('Ctrl Pts',(201.056254175817,88.1909801212834,334.44105583193));
#23966=CARTESIAN_POINT('Ctrl Pts',(199.95737379632,88.2298802575433,335.086005660858));
#23967=CARTESIAN_POINT('Ctrl Pts',(199.471903535416,88.2500471815186,335.513960251011));
#23968=CARTESIAN_POINT('Ctrl Pts',(198.673788261365,88.2927299786094,336.549836946009));
#23969=CARTESIAN_POINT('Ctrl Pts',(198.37666142415,88.3144309354573,337.153766384104));
#23970=CARTESIAN_POINT('Ctrl Pts',(198.043129582088,88.3543991722063,338.418037257362));
#23971=CARTESIAN_POINT('Ctrl Pts',(198.000324105281,88.3745056169959,339.063645207031));
#23972=CARTESIAN_POINT('Ctrl Pts',(198.164036244939,88.4171703698358,340.36065777686));
#23973=CARTESIAN_POINT('Ctrl Pts',(198.378711301086,88.4388754227734,340.998310722234));
#23974=CARTESIAN_POINT('Ctrl Pts',(199.03269180681,88.4788846944295,342.130102793843));
#23975=CARTESIAN_POINT('Ctrl Pts',(199.457114736403,88.4989280935846,342.618284039044));
#23976=CARTESIAN_POINT('Ctrl Pts',(200.486811363997,88.5415733489109,343.423106824859));
#23977=CARTESIAN_POINT('Ctrl Pts',(201.088166405913,88.5632824904017,343.724286290855));
#23978=CARTESIAN_POINT('Ctrl Pts',(202.349249899138,88.6033352439291,344.06676520106));
#23979=CARTESIAN_POINT('Ctrl Pts',(202.994240055269,88.6233131629387,344.114276293583));
#23980=CARTESIAN_POINT('Ctrl Pts',(204.291632762956,88.6659373688183,343.960272214956));
#23981=CARTESIAN_POINT('Ctrl Pts',(204.930381417393,88.6876505466125,343.750592929646));
#23982=CARTESIAN_POINT('Ctrl Pts',(206.066495555729,88.7277492840862,343.105759577051));
#23983=CARTESIAN_POINT('Ctrl Pts',(206.557754177849,88.7476594657781,342.68534264916));
#23984=CARTESIAN_POINT('Ctrl Pts',(207.370150628802,88.7902609688187,341.662675323108));
#23985=CARTESIAN_POINT('Ctrl Pts',(207.675900131243,88.8119780788274,341.064270729581));
#23986=CARTESIAN_POINT('Ctrl Pts',(207.877155278121,88.8348930549401,340.346560173747));
#23987=CARTESIAN_POINT('Ctrl Pts',(207.896880887269,88.8373282945415,340.269104924431));
#23988=CARTESIAN_POINT('Ctrl Pts',(207.914727694784,88.8397376070391,340.191287620971));
#23989=CARTESIAN_POINT('Origin',(203.041252647846,100.739737607039,339.073593133701));
#23990=CARTESIAN_POINT('',(207.91472769442,89.9647376096719,340.191287622561));
#23991=CARTESIAN_POINT('',(207.914727694784,89.8397376070391,340.191287620971));
#23992=CARTESIAN_POINT('',(207.914727694784,100.739737607039,340.191287620971));
#23993=CARTESIAN_POINT('Ctrl Pts',(207.914727694055,89.9647376096719,340.19128762415));
#23994=CARTESIAN_POINT('Ctrl Pts',(207.765836313037,89.9446373276548,340.840497615063));
#23995=CARTESIAN_POINT('Ctrl Pts',(207.488691142175,89.9230721417589,341.453535818966));
#23996=CARTESIAN_POINT('Ctrl Pts',(206.723968003099,89.8803105231624,342.516118973487));
#23997=CARTESIAN_POINT('Ctrl Pts',(206.25123333942,89.859527679405,342.960682232891));
#23998=CARTESIAN_POINT('Ctrl Pts',(205.142071735324,89.8199224731142,343.659758184998));
#23999=CARTESIAN_POINT('Ctrl Pts',(204.511116747618,89.7983389472792,343.899148565792));
#24000=CARTESIAN_POINT('Ctrl Pts',(203.217243112099,89.7555097258034,344.111698106939));
#24001=CARTESIAN_POINT('Ctrl Pts',(202.568513826031,89.7347193400774,344.092562469778));
#24002=CARTESIAN_POINT('Ctrl Pts',(201.289709194899,89.6950996203709,343.804145989652));
#24003=CARTESIAN_POINT('Ctrl Pts',(200.674156782173,89.6735487572462,343.528144091416));
#24004=CARTESIAN_POINT('Ctrl Pts',(199.608064700761,89.6307244318617,342.765042758847));
#24005=CARTESIAN_POINT('Ctrl Pts',(199.162199994239,89.6099259509072,342.293312188139));
#24006=CARTESIAN_POINT('Ctrl Pts',(198.460560629068,89.5702906244146,341.186164222411));
#24007=CARTESIAN_POINT('Ctrl Pts',(198.219699953616,89.5487747405038,340.556311920956));
#24008=CARTESIAN_POINT('Ctrl Pts',(198.003625675874,89.5059557392046,339.263350691311));
#24009=CARTESIAN_POINT('Ctrl Pts',(198.021004392555,89.4851485762116,338.614397131199));
#24010=CARTESIAN_POINT('Ctrl Pts',(198.305934471926,89.4454964780859,337.335175835121));
#24011=CARTESIAN_POINT('Ctrl Pts',(198.579978018731,89.4240180164272,336.719344213792));
#24012=CARTESIAN_POINT('Ctrl Pts',(199.339699623022,89.3812048051796,335.651266291293));
#24013=CARTESIAN_POINT('Ctrl Pts',(199.810260907171,89.360388338936,335.20389445849));
#24014=CARTESIAN_POINT('Ctrl Pts',(200.915070081928,89.3207182299794,334.499285318589));
#24015=CARTESIAN_POINT('Ctrl Pts',(201.543644603275,89.2992797606034,334.25672303268));
#24016=CARTESIAN_POINT('Ctrl Pts',(202.835541442451,89.256472846674,334.036567182181));
#24017=CARTESIAN_POINT('Ctrl Pts',(203.48474907395,89.2356464209134,334.051908390896));
#24018=CARTESIAN_POINT('Ctrl Pts',(204.764447665162,89.1959569849016,334.332799148957));
#24019=CARTESIAN_POINT('Ctrl Pts',(205.380600721626,89.174561203976,334.604577695675));
#24020=CARTESIAN_POINT('Ctrl Pts',(206.450969076925,89.1317611395162,335.36038385866));
#24021=CARTESIAN_POINT('Ctrl Pts',(206.900081924164,89.1109240625106,335.829585646961));
#24022=CARTESIAN_POINT('Ctrl Pts',(207.608123444597,89.0712139037832,336.931683747536));
#24023=CARTESIAN_POINT('Ctrl Pts',(207.852650079897,89.0498636311976,337.558781077251));
#24024=CARTESIAN_POINT('Ctrl Pts',(208.077520715676,89.0070710170895,338.849437926982));
#24025=CARTESIAN_POINT('Ctrl Pts',(208.064537138292,88.9862225615405,339.498931492889));
#24026=CARTESIAN_POINT('Ctrl Pts',(207.92423497449,88.9660411934147,340.149208900489));
#24027=CARTESIAN_POINT('Ctrl Pts',(207.919548623402,88.9653884333734,340.170266961399));
#24028=CARTESIAN_POINT('Ctrl Pts',(207.914727694784,88.9647376097703,340.191287620971));
#24029=CARTESIAN_POINT('Ctrl Pts',(207.914727694784,88.8397376070391,340.191287620971));
#24030=CARTESIAN_POINT('Ctrl Pts',(208.039783122405,88.8566200441031,339.646009360289));
#24031=CARTESIAN_POINT('Ctrl Pts',(208.072570540725,88.8745745972925,339.08302195561));
#24032=CARTESIAN_POINT('Ctrl Pts',(207.938295616732,88.9145428019993,337.864761677801));
#24033=CARTESIAN_POINT('Ctrl Pts',(207.734267589585,88.9362636808166,337.224819805819));
#24034=CARTESIAN_POINT('Ctrl Pts',(207.099781432225,88.9764620461028,336.083865485545));
#24035=CARTESIAN_POINT('Ctrl Pts',(206.683879353213,88.9962309428581,335.589135578386));
#24036=CARTESIAN_POINT('Ctrl Pts',(205.669157623561,89.0387816650799,334.768248217967));
#24037=CARTESIAN_POINT('Ctrl Pts',(205.07411610365,89.0605060822714,334.457383359739));
#24038=CARTESIAN_POINT('Ctrl Pts',(203.820831313731,89.1007581284528,334.093409377673));
#24039=CARTESIAN_POINT('Ctrl Pts',(203.177317914083,89.1204540948528,334.034595137357));
#24040=CARTESIAN_POINT('Ctrl Pts',(201.879157737075,89.1629765301353,334.165338091881));
#24041=CARTESIAN_POINT('Ctrl Pts',(201.23793384196,89.1847041804466,334.363017924715));
#24042=CARTESIAN_POINT('Ctrl Pts',(200.091603706288,89.2250124793616,334.985879532102));
#24043=CARTESIAN_POINT('Ctrl Pts',(199.592985793183,89.244634498187,335.396729857411));
#24044=CARTESIAN_POINT('Ctrl Pts',(198.762654773095,89.2871265777634,336.40253314374));
#24045=CARTESIAN_POINT('Ctrl Pts',(198.446111687749,89.3088570734383,336.993765169786));
#24046=CARTESIAN_POINT('Ctrl Pts',(198.06945739481,89.3492241660787,338.242354716365));
#24047=CARTESIAN_POINT('Ctrl Pts',(198.003974576252,89.3687716758309,338.885001849879));
#24048=CARTESIAN_POINT('Ctrl Pts',(198.121036203777,89.4112312310817,340.183519585841));
#24049=CARTESIAN_POINT('Ctrl Pts',(198.311640785712,89.4329640945147,340.826099870704));
#24050=CARTESIAN_POINT('Ctrl Pts',(198.921542813813,89.4733924677716,341.97834606647));
#24051=CARTESIAN_POINT('Ctrl Pts',(199.326785715225,89.4928654224372,342.481284614558));
#24052=CARTESIAN_POINT('Ctrl Pts',(200.322657070839,89.5352901897899,343.322026523897));
#24053=CARTESIAN_POINT('Ctrl Pts',(200.909604638288,89.5570248467713,343.644814478036));
#24054=CARTESIAN_POINT('Ctrl Pts',(202.152920910627,89.5975169085681,344.035486130514));
#24055=CARTESIAN_POINT('Ctrl Pts',(202.794614536233,89.6169158355446,344.108343155427));
#24056=CARTESIAN_POINT('Ctrl Pts',(204.093446611738,89.6593034633917,344.006370656474));
#24057=CARTESIAN_POINT('Ctrl Pts',(204.737436987694,89.6810392372306,343.823582864136));
#24058=CARTESIAN_POINT('Ctrl Pts',(205.896128026944,89.7215972903815,343.22800597391));
#24059=CARTESIAN_POINT('Ctrl Pts',(206.40382650992,89.740923344727,342.828932689881));
#24060=CARTESIAN_POINT('Ctrl Pts',(207.255934687688,89.7832714025403,341.844025663645));
#24061=CARTESIAN_POINT('Ctrl Pts',(207.585520870882,89.8050075093724,341.261857912909));
#24062=CARTESIAN_POINT('Ctrl Pts',(207.839739270826,89.8304444167043,340.487071034736));
#24063=CARTESIAN_POINT('Ctrl Pts',(207.880650046621,89.8351371369807,340.339876139457));
#24064=CARTESIAN_POINT('Ctrl Pts',(207.914727694784,89.8397376070391,340.191287620971));
#24065=CARTESIAN_POINT('Origin',(203.041252647846,100.739737607039,339.073593133701));
#24066=CARTESIAN_POINT('',(207.914727694784,90.9647376097703,340.191287620971));
#24067=CARTESIAN_POINT('',(207.914727694784,90.8397376070391,340.191287620971));
#24068=CARTESIAN_POINT('',(207.914727694784,100.739737607039,340.191287620971));
#24069=CARTESIAN_POINT('Ctrl Pts',(207.914727694784,90.9647376097703,340.191287620971));
#24070=CARTESIAN_POINT('Ctrl Pts',(207.911315614514,90.9642769801797,340.206165289461));
#24071=CARTESIAN_POINT('Ctrl Pts',(207.907834706666,90.9638153823686,340.221030386257));
#24072=CARTESIAN_POINT('Ctrl Pts',(207.748995822073,90.9431175509878,340.885614180962));
#24073=CARTESIAN_POINT('Ctrl Pts',(207.465064048657,90.9214503419892,341.497658974635));
#24074=CARTESIAN_POINT('Ctrl Pts',(206.688739812019,90.8786533272244,342.55332217813));
#24075=CARTESIAN_POINT('Ctrl Pts',(206.211987656894,90.858050405444,342.992649373643));
#24076=CARTESIAN_POINT('Ctrl Pts',(205.0964906552,90.8183824836142,343.680372545011));
#24077=CARTESIAN_POINT('Ctrl Pts',(204.463211692172,90.7967181428265,343.913467941326));
#24078=CARTESIAN_POINT('Ctrl Pts',(203.167915983234,90.7539132949477,344.113112254686));
#24079=CARTESIAN_POINT('Ctrl Pts',(202.520014328993,90.7332767213144,344.087672267514));
#24080=CARTESIAN_POINT('Ctrl Pts',(201.244282853357,90.6936279488897,343.787133415081));
#24081=CARTESIAN_POINT('Ctrl Pts',(200.631132545857,90.6719663189768,343.50505100369));
#24082=CARTESIAN_POINT('Ctrl Pts',(199.572735897812,90.6291542589892,342.731775884857));
#24083=CARTESIAN_POINT('Ctrl Pts',(199.131829275079,90.6084862284796,342.256233206372));
#24084=CARTESIAN_POINT('Ctrl Pts',(198.440557748886,90.5688552399164,341.142481984388));
#24085=CARTESIAN_POINT('Ctrl Pts',(198.205526680641,90.5471961660466,340.509693352836));
#24086=CARTESIAN_POINT('Ctrl Pts',(198.002092924037,90.5043774669823,339.21460737477));
#24087=CARTESIAN_POINT('Ctrl Pts',(198.025705648113,90.4836800703889,338.566463229518));
#24088=CARTESIAN_POINT('Ctrl Pts',(198.322776246166,90.444065584652,337.289553462054));
#24089=CARTESIAN_POINT('Ctrl Pts',(198.603268531205,90.4224089156099,336.675458761662));
#24090=CARTESIAN_POINT('Ctrl Pts',(199.373922787544,90.3795841059849,335.614719441325));
#24091=CARTESIAN_POINT('Ctrl Pts',(199.848427824991,90.3588593286175,335.172457490587));
#24092=CARTESIAN_POINT('Ctrl Pts',(200.960678185243,90.3192601458917,334.478145342542));
#24093=CARTESIAN_POINT('Ctrl Pts',(201.593042050042,90.2976057349498,334.241455871552));
#24094=CARTESIAN_POINT('Ctrl Pts',(202.887943831758,90.2547753020222,334.034773284165));
#24095=CARTESIAN_POINT('Ctrl Pts',(203.536295954121,90.234025023694,334.056819976455));
#24096=CARTESIAN_POINT('Ctrl Pts',(204.814211375342,90.1944400219056,334.350918809372));
#24097=CARTESIAN_POINT('Ctrl Pts',(205.429111504593,90.1727877274885,334.630047356649));
#24098=CARTESIAN_POINT('Ctrl Pts',(206.49179462128,90.1299545299613,335.398411252325));
#24099=CARTESIAN_POINT('Ctrl Pts',(206.935236426321,90.1091852393959,335.872006985988));
#24100=CARTESIAN_POINT('Ctrl Pts',(207.632104259007,90.0696060505826,336.982899331542));
#24101=CARTESIAN_POINT('Ctrl Pts',(207.870226988821,90.0479636513252,337.614803975402));
#24102=CARTESIAN_POINT('Ctrl Pts',(208.079739104538,90.005125784942,338.909458833918));
#24103=CARTESIAN_POINT('Ctrl Pts',(208.059091403677,89.9843499624347,339.557991247767));
#24104=CARTESIAN_POINT('Ctrl Pts',(207.915713008852,89.9648708373616,340.186984826092));
#24105=CARTESIAN_POINT('Ctrl Pts',(207.915221055665,89.9648042133088,340.189136423161));
#24106=CARTESIAN_POINT('Ctrl Pts',(207.914727694055,89.9647376096719,340.19128762415));
#24107=CARTESIAN_POINT('Ctrl Pts',(207.914727694784,89.8397376070391,340.191287620971));
#24108=CARTESIAN_POINT('Ctrl Pts',(208.023215162931,89.854383375624,339.718250512049));
#24109=CARTESIAN_POINT('Ctrl Pts',(208.062435766932,89.8698590586585,339.231140777883));
#24110=CARTESIAN_POINT('Ctrl Pts',(207.986989240129,89.9071947273622,338.084683157661));
#24111=CARTESIAN_POINT('Ctrl Pts',(207.812754309931,89.9289302729595,337.439255866093));
#24112=CARTESIAN_POINT('Ctrl Pts',(207.232863968651,89.969626661502,336.273621397437));
#24113=CARTESIAN_POINT('Ctrl Pts',(206.84051399295,89.9888131813776,335.7607285162));
#24114=CARTESIAN_POINT('Ctrl Pts',(205.867595136952,90.0310745515505,334.896341406658));
#24115=CARTESIAN_POINT('Ctrl Pts',(205.290711644538,90.0528085299448,334.559436652983));
#24116=CARTESIAN_POINT('Ctrl Pts',(204.059760957976,90.093576916516,334.136778324456));
#24117=CARTESIAN_POINT('Ctrl Pts',(203.420228210987,90.1126982392496,334.047074883442));
#24118=CARTESIAN_POINT('Ctrl Pts',(202.120991259532,90.1549124009898,334.114749265968));
#24119=CARTESIAN_POINT('Ctrl Pts',(201.474132624673,90.1766436952053,334.279724492657));
#24120=CARTESIAN_POINT('Ctrl Pts',(200.301106772013,90.217485691699,334.842612445414));
#24121=CARTESIAN_POINT('Ctrl Pts',(199.782603329716,90.2365458797191,335.227711231833));
#24122=CARTESIAN_POINT('Ctrl Pts',(198.905101251835,90.278710225717,336.187659101803));
#24123=CARTESIAN_POINT('Ctrl Pts',(198.560411951696,90.3004376108674,336.758759251106));
#24124=CARTESIAN_POINT('Ctrl Pts',(198.119921305086,90.3413545916701,337.982611312581));
#24125=CARTESIAN_POINT('Ctrl Pts',(198.02080853357,90.3603584786334,338.620947320342));
#24126=CARTESIAN_POINT('Ctrl Pts',(198.069441093885,90.4024704041232,339.920224927786));
#24127=CARTESIAN_POINT('Ctrl Pts',(198.224505503012,90.4241925530731,340.568472890227));
#24128=CARTESIAN_POINT('Ctrl Pts',(198.769167220228,90.4651856326072,341.749266742395));
#24129=CARTESIAN_POINT('Ctrl Pts',(199.146531472698,90.4841388126341,342.27376378772));
#24130=CARTESIAN_POINT('Ctrl Pts',(200.092602516096,90.5261957384747,343.165105483259));
#24131=CARTESIAN_POINT('Ctrl Pts',(200.6574427396,90.5479112301913,343.517969530997));
#24132=CARTESIAN_POINT('Ctrl Pts',(201.873612083517,90.5889812433873,343.977348334716));
#24133=CARTESIAN_POINT('Ctrl Pts',(202.510685454206,90.6078900436021,344.086446491198));
#24134=CARTESIAN_POINT('Ctrl Pts',(203.809864421873,90.6498894410831,344.057923331698));
#24135=CARTESIAN_POINT('Ctrl Pts',(204.459421447231,90.6715967717128,343.913337592328));
#24136=CARTESIAN_POINT('Ctrl Pts',(205.648269371093,90.7127442580518,343.387985290973));
#24137=CARTESIAN_POINT('Ctrl Pts',(206.17909464918,90.7316156938061,343.018775424987));
#24138=CARTESIAN_POINT('Ctrl Pts',(207.084856353885,90.7735551107592,342.087372923418));
#24139=CARTESIAN_POINT('Ctrl Pts',(207.446189989066,90.7952527073595,341.529227748421));
#24140=CARTESIAN_POINT('Ctrl Pts',(207.782744424956,90.8242100641158,340.680741423644));
#24141=CARTESIAN_POINT('Ctrl Pts',(207.85812863934,90.8320967552217,340.438076065871));
#24142=CARTESIAN_POINT('Ctrl Pts',(207.914727694784,90.8397376070391,340.191287620971));
#24143=CARTESIAN_POINT('Origin',(203.041252647846,100.739737607039,339.073593133701));
#24144=CARTESIAN_POINT('',(207.914727694784,91.9647376097702,340.191287620971));
#24145=CARTESIAN_POINT('',(207.914727694784,91.8397376070391,340.191287620971));
#24146=CARTESIAN_POINT('',(207.914727694784,100.739737607039,340.191287620971));
#24147=CARTESIAN_POINT('Ctrl Pts',(207.914727694784,91.9647376097703,340.191287620971));
#24148=CARTESIAN_POINT('Ctrl Pts',(207.904254565996,91.9633237412082,340.236953527346));
#24149=CARTESIAN_POINT('Ctrl Pts',(207.893133690911,91.9619008454671,340.282497930865));
#24150=CARTESIAN_POINT('Ctrl Pts',(207.714105944956,91.940122244649,340.973325472129));
#24151=CARTESIAN_POINT('Ctrl Pts',(207.419431766777,91.9184267450767,341.57879400991));
#24152=CARTESIAN_POINT('Ctrl Pts',(206.625372232688,91.8757217952659,342.61838696805));
#24153=CARTESIAN_POINT('Ctrl Pts',(206.141534760899,91.8554776998392,343.048469769076));
#24154=CARTESIAN_POINT('Ctrl Pts',(205.015891675147,91.815596502115,343.715318372967));
#24155=CARTESIAN_POINT('Ctrl Pts',(204.379845146041,91.7939049779004,343.937020373372));
#24156=CARTESIAN_POINT('Ctrl Pts',(203.083428523973,91.7511850254589,344.114413409457));
#24157=CARTESIAN_POINT('Ctrl Pts',(202.436948534698,91.730886764099,344.078228661387));
#24158=CARTESIAN_POINT('Ctrl Pts',(201.168252151569,91.6910389414042,343.757281372481));
#24159=CARTESIAN_POINT('Ctrl Pts',(200.560755003687,91.6693512961696,343.46587485997));
#24160=CARTESIAN_POINT('Ctrl Pts',(199.516238464375,91.6266174911885,342.677214788824));
#24161=CARTESIAN_POINT('Ctrl Pts',(199.083330651644,91.6062677997654,342.195543722738));
#24162=CARTESIAN_POINT('Ctrl Pts',(198.410083905223,91.5664512462118,341.072987920166));
#24163=CARTESIAN_POINT('Ctrl Pts',(198.184888851631,91.5447673641103,340.43776840419));
#24164=CARTESIAN_POINT('Ctrl Pts',(198.000683309217,91.5020207752774,339.141674950375));
#24165=CARTESIAN_POINT('Ctrl Pts',(198.033575491245,91.4816223761694,338.494760123088));
#24166=CARTESIAN_POINT('Ctrl Pts',(198.348266638407,91.4418350779639,337.223888606625));
#24167=CARTESIAN_POINT('Ctrl Pts',(198.636820966877,91.4201548280399,336.614641057529));
#24168=CARTESIAN_POINT('Ctrl Pts',(199.420771582785,91.3773964471176,335.565852361434));
#24169=CARTESIAN_POINT('Ctrl Pts',(199.900559811442,91.3569520271025,335.130488175659));
#24170=CARTESIAN_POINT('Ctrl Pts',(201.020421611829,91.3171920645888,334.451691747877));
#24171=CARTESIAN_POINT('Ctrl Pts',(201.654908567266,91.295515304612,334.223467461566));
#24172=CARTESIAN_POINT('Ctrl Pts',(202.950707148227,91.2527460509195,334.03334736297));
#24173=CARTESIAN_POINT('Ctrl Pts',(203.597999806697,91.2322582427972,334.063383117562));
#24174=CARTESIAN_POINT('Ctrl Pts',(204.870744491466,91.192523791354,334.372648356914));
#24175=CARTESIAN_POINT('Ctrl Pts',(205.481497664974,91.1708503711545,334.658724598177));
#24176=CARTESIAN_POINT('Ctrl Pts',(206.533979223132,91.1280710959943,335.438585899667));
#24177=CARTESIAN_POINT('Ctrl Pts',(206.971470652013,91.1075424636214,335.916744200083));
#24178=CARTESIAN_POINT('Ctrl Pts',(207.655062876658,91.0678317935738,337.034265884231));
#24179=CARTESIAN_POINT('Ctrl Pts',(207.88590435845,91.0461615579108,337.668108405244));
#24180=CARTESIAN_POINT('Ctrl Pts',(208.078863787454,91.003871830217,338.948539322099));
#24181=CARTESIAN_POINT('Ctrl Pts',(208.054814952644,90.9836493384277,339.580466181525));
#24182=CARTESIAN_POINT('Ctrl Pts',(207.914727694784,90.9647376097703,340.191287620971));
#24183=CARTESIAN_POINT('Ctrl Pts',(207.914727694784,90.8397376070391,340.191287620971));
#24184=CARTESIAN_POINT('Ctrl Pts',(208.00079559222,90.8513567417646,339.816006401218));
#24185=CARTESIAN_POINT('Ctrl Pts',(208.04341648959,90.8635181561768,339.431223786886));
#24186=CARTESIAN_POINT('Ctrl Pts',(208.037342853879,90.8971966995547,338.386599953585));
#24187=CARTESIAN_POINT('Ctrl Pts',(207.903693993538,90.9188829362989,337.73585134799));
#24188=CARTESIAN_POINT('Ctrl Pts',(207.398546275849,90.9601857510994,336.538769603378));
#24189=CARTESIAN_POINT('Ctrl Pts',(207.037829385965,90.9790059298629,336.001344521028));
#24190=CARTESIAN_POINT('Ctrl Pts',(206.121737554768,91.0208184701916,335.080754684404));
#24191=CARTESIAN_POINT('Ctrl Pts',(205.570661670986,91.042491686754,334.710767762962));
#24192=CARTESIAN_POINT('Ctrl Pts',(204.37140152303,91.0838717256542,334.211232479903));
#24193=CARTESIAN_POINT('Ctrl Pts',(203.737001858586,91.1026790128869,334.080820427013));
#24194=CARTESIAN_POINT('Ctrl Pts',(202.438507526252,91.1444249449932,334.066786989316));
#24195=CARTESIAN_POINT('Ctrl Pts',(201.786717910239,91.1660834667067,334.1891731859));
#24196=CARTESIAN_POINT('Ctrl Pts',(200.581339502808,91.2075400168075,334.673451125967));
#24197=CARTESIAN_POINT('Ctrl Pts',(200.037118864543,91.2263434015514,335.025432819567));
#24198=CARTESIAN_POINT('Ctrl Pts',(199.101485417345,91.2680208475195,335.925752043778));
#24199=CARTESIAN_POINT('Ctrl Pts',(198.722782861348,91.2896630068129,336.469463462791));
#24200=CARTESIAN_POINT('Ctrl Pts',(198.20246699672,91.3311950492952,337.659656524762));
#24201=CARTESIAN_POINT('Ctrl Pts',(198.060968683261,91.3500037497455,338.292674017094));
#24202=CARTESIAN_POINT('Ctrl Pts',(198.025012185414,91.3916110384711,339.590565086089));
#24203=CARTESIAN_POINT('Ctrl Pts',(198.135959196406,91.4132351970082,340.243219103971));
#24204=CARTESIAN_POINT('Ctrl Pts',(198.59896480335,91.4548414274877,341.456836241764));
#24205=CARTESIAN_POINT('Ctrl Pts',(198.94207630356,91.473664751609,342.007962310047));
#24206=CARTESIAN_POINT('Ctrl Pts',(199.826364104401,91.515200448587,342.95865178267));
#24207=CARTESIAN_POINT('Ctrl Pts',(200.362510056219,91.5368050177093,343.346007517477));
#24208=CARTESIAN_POINT('Ctrl Pts',(201.543367467538,91.5784838632738,343.887206904971));
#24209=CARTESIAN_POINT('Ctrl Pts',(202.174991719712,91.59733108359,344.039892574598));
#24210=CARTESIAN_POINT('Ctrl Pts',(203.472109271237,91.6387940062626,344.097816099371));
#24211=CARTESIAN_POINT('Ctrl Pts',(204.125434244662,91.6603774719498,343.998326498988));
#24212=CARTESIAN_POINT('Ctrl Pts',(205.347115042016,91.7021270925556,343.556713039399));
#24213=CARTESIAN_POINT('Ctrl Pts',(205.90516388146,91.7210073554214,343.222494051428));
#24214=CARTESIAN_POINT('Ctrl Pts',(206.870719457898,91.7623965702574,342.354280424769));
#24215=CARTESIAN_POINT('Ctrl Pts',(207.266544924304,91.7839575123391,341.825796270456));
#24216=CARTESIAN_POINT('Ctrl Pts',(207.709836503838,91.8169485008814,340.901684117415));
#24217=CARTESIAN_POINT('Ctrl Pts',(207.832182807031,91.8285940773342,340.551207487534));
#24218=CARTESIAN_POINT('Ctrl Pts',(207.914727694784,91.8397376070391,340.191287620971));
#24219=CARTESIAN_POINT('Origin',(203.041252647846,100.739737607039,339.073593133701));
#24220=CARTESIAN_POINT('',(207.914727694784,92.9647376097703,340.191287620971));
#24221=CARTESIAN_POINT('',(207.914727694784,92.8397376070391,340.191287620971));
#24222=CARTESIAN_POINT('',(207.914727694784,100.739737607039,340.191287620971));
#24223=CARTESIAN_POINT('Ctrl Pts',(207.914727694784,92.9647376097703,340.191287620971));
#24224=CARTESIAN_POINT('Ctrl Pts',(207.892227982976,92.9617001568921,340.289392948778));
#24225=CARTESIAN_POINT('Ctrl Pts',(207.866744237917,92.9586217814126,340.386913603745));
#24226=CARTESIAN_POINT('Ctrl Pts',(207.650868691199,92.9349863231015,341.121293124528));
#24227=CARTESIAN_POINT('Ctrl Pts',(207.338208134411,92.9132597503841,341.715138681599));
#24228=CARTESIAN_POINT('Ctrl Pts',(206.514336473059,92.8707273127763,342.727051367469));
#24229=CARTESIAN_POINT('Ctrl Pts',(206.018381055642,92.8510060114433,343.141360532428));
#24230=CARTESIAN_POINT('Ctrl Pts',(204.875727022238,92.8107728045649,343.772186534325));
#24231=CARTESIAN_POINT('Ctrl Pts',(204.235374813868,92.7890495793809,343.974215619768));
#24232=CARTESIAN_POINT('Ctrl Pts',(202.93746924036,92.7464895458046,344.113380838905));
#24233=CARTESIAN_POINT('Ctrl Pts',(202.293421719787,92.7266957605897,344.058664024676));
#24234=CARTESIAN_POINT('Ctrl Pts',(201.03728664979,92.6865153427722,343.702482201109));
#24235=CARTESIAN_POINT('Ctrl Pts',(200.43993545088,92.6647957436461,343.395119864489));
#24236=CARTESIAN_POINT('Ctrl Pts',(199.41976437803,92.6222100439426,342.580047896261));
#24237=CARTESIAN_POINT('Ctrl Pts',(199.000767362234,92.6023453107654,342.087697910815));
#24238=CARTESIAN_POINT('Ctrl Pts',(198.359183863117,92.5622151020548,340.950057974279));
#24239=CARTESIAN_POINT('Ctrl Pts',(198.151279548677,92.540499335381,340.310929267508));
#24240=CARTESIAN_POINT('Ctrl Pts',(198.000721208541,92.4978897947837,339.013410133542));
#24241=CARTESIAN_POINT('Ctrl Pts',(198.049904086809,92.4779559666251,338.368639047898));
#24242=CARTESIAN_POINT('Ctrl Pts',(198.395562021898,92.4378734031648,337.108696346758));
#24243=CARTESIAN_POINT('Ctrl Pts',(198.69817850748,92.4161616109913,336.508263606751));
#24244=CARTESIAN_POINT('Ctrl Pts',(199.505381623403,92.3735299504441,335.48077035533));
#24245=CARTESIAN_POINT('Ctrl Pts',(199.994528170868,92.3535291417961,335.057604361251));
#24246=CARTESIAN_POINT('Ctrl Pts',(201.127679077017,92.3134916923056,334.406490428141));
#24247=CARTESIAN_POINT('Ctrl Pts',(201.765679529091,92.2917839599802,334.193380929935));
#24248=CARTESIAN_POINT('Ctrl Pts',(203.062815096665,92.2491317975486,334.032712656847));
#24249=CARTESIAN_POINT('Ctrl Pts',(203.708229251426,92.2290663322601,334.076992835882));
#24250=CARTESIAN_POINT('Ctrl Pts',(204.97150497861,92.1890715123517,334.413328425462));
#24251=CARTESIAN_POINT('Ctrl Pts',(205.574631065039,92.1673678758902,334.711726536329));
#24252=CARTESIAN_POINT('Ctrl Pts',(206.608574463218,92.1246967290659,335.511945063808));
#24253=CARTESIAN_POINT('Ctrl Pts',(207.03542325672,92.1045690921455,335.998263962301));
#24254=CARTESIAN_POINT('Ctrl Pts',(207.694927150099,92.0646144765212,337.12742654897));
#24255=CARTESIAN_POINT('Ctrl Pts',(207.912618599103,92.0429149295889,337.764399278767));
#24256=CARTESIAN_POINT('Ctrl Pts',(208.076116420636,92.0017575456216,339.014647340122));
#24257=CARTESIAN_POINT('Ctrl Pts',(208.047426427959,91.9826518902931,339.612682311334));
#24258=CARTESIAN_POINT('Ctrl Pts',(207.914727694784,91.9647376097703,340.191287620971));
#24259=CARTESIAN_POINT('Ctrl Pts',(207.914727694784,91.8397376070391,340.191287620971));
#24260=CARTESIAN_POINT('Ctrl Pts',(207.975755026631,91.8479762745539,339.925190595062));
#24261=CARTESIAN_POINT('Ctrl Pts',(208.015023379492,91.8564989753866,339.65394854609));
#24262=CARTESIAN_POINT('Ctrl Pts',(208.071915560571,91.8860128619997,338.727998026453));
#24263=CARTESIAN_POINT('Ctrl Pts',(207.98374299771,91.9075499725715,338.074201598698));
#24264=CARTESIAN_POINT('Ctrl Pts',(207.563354323306,91.9494347389235,336.844741368962));
#24265=CARTESIAN_POINT('Ctrl Pts',(207.237935160857,91.9684073028415,336.279842850259));
#24266=CARTESIAN_POINT('Ctrl Pts',(206.385622568559,92.009647402592,335.299803740156));
#24267=CARTESIAN_POINT('Ctrl Pts',(205.864787174727,92.0311595024063,334.8958023824));
#24268=CARTESIAN_POINT('Ctrl Pts',(204.702911587947,92.0731082695322,334.31365047058));
#24269=CARTESIAN_POINT('Ctrl Pts',(204.074041625411,92.0921391997607,334.138867997609));
#24270=CARTESIAN_POINT('Ctrl Pts',(202.778922520765,92.133304456027,334.038041146075));
#24271=CARTESIAN_POINT('Ctrl Pts',(202.124849705415,92.1547905081741,334.115187128895));
#24272=CARTESIAN_POINT('Ctrl Pts',(200.88798696223,92.1968006991891,334.514795833626));
#24273=CARTESIAN_POINT('Ctrl Pts',(200.31640011974,92.2158973817219,334.831616638204));
#24274=CARTESIAN_POINT('Ctrl Pts',(199.322431386889,92.2569879799097,335.668407568756));
#24275=CARTESIAN_POINT('Ctrl Pts',(198.910642365424,92.2784471004846,336.181714864627));
#24276=CARTESIAN_POINT('Ctrl Pts',(198.308941897931,92.3205160311824,337.334203367042));
#24277=CARTESIAN_POINT('Ctrl Pts',(198.123526783317,92.3396851833687,337.96174198073));
#24278=CARTESIAN_POINT('Ctrl Pts',(198.002294507203,92.3807015847452,339.255684549381));
#24279=CARTESIAN_POINT('Ctrl Pts',(198.068838247974,92.4021330503188,339.909852568494));
#24280=CARTESIAN_POINT('Ctrl Pts',(198.448365079681,92.4442579602656,341.15366757279));
#24281=CARTESIAN_POINT('Ctrl Pts',(198.756887665259,92.4635055704234,341.731701476214));
#24282=CARTESIAN_POINT('Ctrl Pts',(199.578721882776,92.5044485024553,342.738902330108));
#24283=CARTESIAN_POINT('Ctrl Pts',(200.084721682248,92.5258517542947,343.158016148845));
#24284=CARTESIAN_POINT('Ctrl Pts',(201.228058569042,92.5680298368164,343.778352321079));
#24285=CARTESIAN_POINT('Ctrl Pts',(201.85431352362,92.5873611212353,343.973960747681));
#24286=CARTESIAN_POINT('Ctrl Pts',(203.147001786061,92.628231564393,344.114605122069));
#24287=CARTESIAN_POINT('Ctrl Pts',(203.801105129643,92.6496062094924,344.058127463367));
#24288=CARTESIAN_POINT('Ctrl Pts',(205.051370084647,92.6918346399555,343.697766670287));
#24289=CARTESIAN_POINT('Ctrl Pts',(205.635541779686,92.711254017264,343.397157636541));
#24290=CARTESIAN_POINT('Ctrl Pts',(206.655165884056,92.7520531887422,342.589558218914));
#24291=CARTESIAN_POINT('Ctrl Pts',(207.081088435159,92.7733989978353,342.090558066796));
#24292=CARTESIAN_POINT('Ctrl Pts',(207.634658915025,92.8100866730409,341.105996354396));
#24293=CARTESIAN_POINT('Ctrl Pts',(207.807904347327,92.8253164941396,340.657068676701));
#24294=CARTESIAN_POINT('Ctrl Pts',(207.914727694784,92.8397376070391,340.191287620971));
#24295=CARTESIAN_POINT('Origin',(203.041252647846,100.739737607039,339.073593133701));
#24296=CARTESIAN_POINT('',(207.914727694784,93.9647376097703,340.191287620971));
#24297=CARTESIAN_POINT('',(207.914727694784,93.8397376070391,340.191287620971));
#24298=CARTESIAN_POINT('',(207.914727694784,100.739737607039,340.191287620971));
#24299=CARTESIAN_POINT('Ctrl Pts',(207.914727694784,93.9647376097703,340.191287620971));
#24300=CARTESIAN_POINT('Ctrl Pts',(207.873804939263,93.9592130527181,340.369722810693));
#24301=CARTESIAN_POINT('Ctrl Pts',(207.823038515332,93.9535568412456,340.546103814389));
#24302=CARTESIAN_POINT('Ctrl Pts',(207.544859034738,93.9270509333428,341.344009870334));
#24303=CARTESIAN_POINT('Ctrl Pts',(207.205454880507,93.9053185785856,341.9190550229));
#24304=CARTESIAN_POINT('Ctrl Pts',(206.336863308448,93.8630878112972,342.887834418589));
#24305=CARTESIAN_POINT('Ctrl Pts',(205.822178923424,93.8439443821288,343.277867828257));
#24306=CARTESIAN_POINT('Ctrl Pts',(204.654171934117,93.8032010656026,343.85233561752));
#24307=CARTESIAN_POINT('Ctrl Pts',(204.008273922891,93.78146642501,344.023616034488));
#24308=CARTESIAN_POINT('Ctrl Pts',(202.709131222029,93.7391893468591,344.103418851654));
#24309=CARTESIAN_POINT('Ctrl Pts',(202.0688352615,93.7199794957506,344.019686859139));
#24310=CARTESIAN_POINT('Ctrl Pts',(200.833450820258,93.679307569546,343.608359267027));
#24311=CARTESIAN_POINT('Ctrl Pts',(200.25295671188,93.6575717219641,343.276433212799));
#24312=CARTESIAN_POINT('Ctrl Pts',(199.271861312971,93.6152509109054,342.420404293397));
#24313=CARTESIAN_POINT('Ctrl Pts',(198.874928115931,93.5959716030076,341.911053208444));
#24314=CARTESIAN_POINT('Ctrl Pts',(198.284335982435,93.5553691749377,340.750142830051));
#24315=CARTESIAN_POINT('Ctrl Pts',(198.104266929115,93.5336330876967,340.105683711802));
#24316=CARTESIAN_POINT('Ctrl Pts',(198.00753666247,93.4912710785197,338.806761983362));
#24317=CARTESIAN_POINT('Ctrl Pts',(198.08296068611,93.4719200173456,338.165399182987));
#24318=CARTESIAN_POINT('Ctrl Pts',(198.478510104806,93.4313850179656,336.92393853915));
#24319=CARTESIAN_POINT('Ctrl Pts',(198.803462998129,93.4096495469072,336.338499897794));
#24320=CARTESIAN_POINT('Ctrl Pts',(199.64782067779,93.3672488157421,335.346102693374));
#24321=CARTESIAN_POINT('Ctrl Pts',(200.152268500491,93.3478244087075,334.942816948992));
#24322=CARTESIAN_POINT('Ctrl Pts',(201.306566580844,93.3073546185777,334.337451817897));
#24323=CARTESIAN_POINT('Ctrl Pts',(201.949603581291,93.2856205100925,334.149323412115));
#24324=CARTESIAN_POINT('Ctrl Pts',(203.248230013819,93.2431834613731,334.037044497523));
#24325=CARTESIAN_POINT('Ctrl Pts',(203.890574709682,93.2236847761094,334.104862394107));
#24326=CARTESIAN_POINT('Ctrl Pts',(205.137503667319,93.18327785308,334.485956033074));
#24327=CARTESIAN_POINT('Ctrl Pts',(205.727387109702,93.1615457478529,334.804480598285));
#24328=CARTESIAN_POINT('Ctrl Pts',(206.73005323215,93.1190747036848,335.638112022245));
#24329=CARTESIAN_POINT('Ctrl Pts',(207.139130334014,93.0995014172781,336.138095670888));
#24330=CARTESIAN_POINT('Ctrl Pts',(207.757900090983,93.059154923242,337.28630252403));
#24331=CARTESIAN_POINT('Ctrl Pts',(207.95334570219,93.037425361389,337.927962978038));
#24332=CARTESIAN_POINT('Ctrl Pts',(208.069986967232,92.998210224646,339.125819186543));
#24333=CARTESIAN_POINT('Ctrl Pts',(208.034997750192,92.980974023333,339.666874983528));
#24334=CARTESIAN_POINT('Ctrl Pts',(207.914727694784,92.9647376097703,340.191287620971));
#24335=CARTESIAN_POINT('Ctrl Pts',(207.914727694784,92.8397376070391,340.191287620971));
#24336=CARTESIAN_POINT('Ctrl Pts',(207.953046404109,92.8449106188056,340.024206834718));
#24337=CARTESIAN_POINT('Ctrl Pts',(207.982817119989,92.8501997477775,339.854964028943));
#24338=CARTESIAN_POINT('Ctrl Pts',(208.08314124294,92.8759153768596,339.039608838099));
#24339=CARTESIAN_POINT('Ctrl Pts',(208.036107293269,92.8972322796717,338.385703867311));
#24340=CARTESIAN_POINT('Ctrl Pts',(207.693822250953,92.9395529881538,337.129522094079));
#24341=CARTESIAN_POINT('Ctrl Pts',(207.400674455767,92.9591585874978,336.539575623612));
#24342=CARTESIAN_POINT('Ctrl Pts',(206.606464645449,92.9998197178356,335.508414682625));
#24343=CARTESIAN_POINT('Ctrl Pts',(206.114085262997,93.0211077959075,335.076231426297));
#24344=CARTESIAN_POINT('Ctrl Pts',(204.987923137303,93.0634705184885,334.421989120271));
#24345=CARTESIAN_POINT('Ctrl Pts',(204.364051254315,93.0831726677721,334.207677672862));
#24346=CARTESIAN_POINT('Ctrl Pts',(203.073975604662,93.1237674003411,334.031805317889));
#24347=CARTESIAN_POINT('Ctrl Pts',(202.420374276277,93.145026877801,334.070077356855));
#24348=CARTESIAN_POINT('Ctrl Pts',(201.158820074663,93.187428952141,334.395504361998));
#24349=CARTESIAN_POINT('Ctrl Pts',(200.563500273469,93.2072289376568,334.681692667663));
#24350=CARTESIAN_POINT('Ctrl Pts',(199.521733604888,93.2477592306827,335.463445609985));
#24351=CARTESIAN_POINT('Ctrl Pts',(199.083850134906,93.2689904633737,335.949636063369));
#24352=CARTESIAN_POINT('Ctrl Pts',(198.41453404593,93.3114293120859,337.067938843608));
#24353=CARTESIAN_POINT('Ctrl Pts',(198.191837186309,93.3313277163342,337.690726855008));
#24354=CARTESIAN_POINT('Ctrl Pts',(198.000336637975,93.3717956559147,338.979504392752));
#24355=CARTESIAN_POINT('Ctrl Pts',(198.030562126869,93.392999119289,339.632725119442));
#24356=CARTESIAN_POINT('Ctrl Pts',(198.340429254254,93.4354722618472,340.899112857338));
#24357=CARTESIAN_POINT('Ctrl Pts',(198.620191065518,93.455469014206,341.499381269254));
#24358=CARTESIAN_POINT('Ctrl Pts',(199.390472404057,93.4958767908359,342.550807705861));
#24359=CARTESIAN_POINT('Ctrl Pts',(199.870940433053,93.517053067019,342.993835149602));
#24360=CARTESIAN_POINT('Ctrl Pts',(200.981943010181,93.5595581289031,343.676915049404));
#24361=CARTESIAN_POINT('Ctrl Pts',(201.603725719806,93.5796525620978,343.907309212695));
#24362=CARTESIAN_POINT('Ctrl Pts',(202.89124454375,93.6200024477401,344.113064218841));
#24363=CARTESIAN_POINT('Ctrl Pts',(203.544034043296,93.641152212143,344.090159679816));
#24364=CARTESIAN_POINT('Ctrl Pts',(204.814735265088,93.6836869314197,343.794517611611));
#24365=CARTESIAN_POINT('Ctrl Pts',(205.41951827782,93.7038778417882,343.5206350808));
#24366=CARTESIAN_POINT('Ctrl Pts',(206.479669165915,93.7441721678624,342.760819666309));
#24367=CARTESIAN_POINT('Ctrl Pts',(206.927301992097,93.7652961756821,342.285590081629));
#24368=CARTESIAN_POINT('Ctrl Pts',(207.572078650103,93.804752097779,341.261893830787));
#24369=CARTESIAN_POINT('Ctrl Pts',(207.789164667609,93.8227866442205,340.738779164257));
#24370=CARTESIAN_POINT('Ctrl Pts',(207.914727694784,93.8397376070391,340.191287620971));
#24371=CARTESIAN_POINT('Origin',(203.041252647846,100.739737607039,339.073593133701));
#24372=CARTESIAN_POINT('',(207.914727694784,94.9647376097703,340.191287620971));
#24373=CARTESIAN_POINT('',(207.914727694784,94.8397376070391,340.191287620971));
#24374=CARTESIAN_POINT('',(207.914727694784,100.739737607039,340.191287620971));
#24375=CARTESIAN_POINT('Ctrl Pts',(207.914727694784,94.9647376097703,340.191287620971));
#24376=CARTESIAN_POINT('Ctrl Pts',(207.849665529396,94.9559542412007,340.474977701877));
#24377=CARTESIAN_POINT('Ctrl Pts',(207.759811904417,94.9468502670507,340.753082234696));
#24378=CARTESIAN_POINT('Ctrl Pts',(207.389785636598,94.9165716596823,341.627400591467));
#24379=CARTESIAN_POINT('Ctrl Pts',(207.016947381176,94.894907871297,342.17609468672));
#24380=CARTESIAN_POINT('Ctrl Pts',(206.091448578882,94.8531387028617,343.087066397982));
#24381=CARTESIAN_POINT('Ctrl Pts',(205.551817251161,94.8343279625663,343.444946375562));
#24382=CARTESIAN_POINT('Ctrl Pts',(204.352021531765,94.7929745410165,343.943325616105));
#24383=CARTESIAN_POINT('Ctrl Pts',(203.700914252711,94.7712966367118,344.07331772725));
#24384=CARTESIAN_POINT('Ctrl Pts',(202.40211293344,94.7294615526946,344.07386083302));
#24385=CARTESIAN_POINT('Ctrl Pts',(201.766796617286,94.7106348898926,343.950778730699));
#24386=CARTESIAN_POINT('Ctrl Pts',(200.561643350943,94.6693588660483,343.46502551495));
#24387=CARTESIAN_POINT('Ctrl Pts',(200.005773851085,94.6476685179065,343.100874619319));
#24388=CARTESIAN_POINT('Ctrl Pts',(199.079319175464,94.6057696364642,342.19029639937));
#24389=CARTESIAN_POINT('Ctrl Pts',(198.712855715638,94.5869185538863,341.657337824743));
#24390=CARTESIAN_POINT('Ctrl Pts',(198.194027083786,94.5457202173699,340.465809699669));
#24391=CARTESIAN_POINT('Ctrl Pts',(198.052975944774,94.5240190759957,339.815848082118));
#24392=CARTESIAN_POINT('Ctrl Pts',(198.031231811742,94.4820586634371,338.51673499509));
#24393=CARTESIAN_POINT('Ctrl Pts',(198.143708038422,94.4631751514099,337.880087191142));
#24394=CARTESIAN_POINT('Ctrl Pts',(198.60946696214,94.4220544753107,336.666551603344));
#24395=CARTESIAN_POINT('Ctrl Pts',(198.965075297147,94.4003441502341,336.10385695742));
#24396=CARTESIAN_POINT('Ctrl Pts',(199.86107981855,94.3583245940889,335.162505522918));
#24397=CARTESIAN_POINT('Ctrl Pts',(200.387613677733,94.3394012193826,334.787767126957));
#24398=CARTESIAN_POINT('Ctrl Pts',(201.571016569693,94.298357864262,334.249313254273));
#24399=CARTESIAN_POINT('Ctrl Pts',(202.21970361048,94.2766399062661,334.097620224748));
#24400=CARTESIAN_POINT('Ctrl Pts',(203.518965300925,94.2345636881629,334.055459895413));
#24401=CARTESIAN_POINT('Ctrl Pts',(204.15689484424,94.2155936670697,334.157780847878));
#24402=CARTESIAN_POINT('Ctrl Pts',(205.378295284628,94.1746269898073,334.604344431639));
#24403=CARTESIAN_POINT('Ctrl Pts',(205.947397761897,94.1529028755505,334.95167017361));
#24404=CARTESIAN_POINT('Ctrl Pts',(206.902899459118,94.1107725445201,335.833627778178));
#24405=CARTESIAN_POINT('Ctrl Pts',(207.285517675167,94.0917497990019,336.35405246242));
#24406=CARTESIAN_POINT('Ctrl Pts',(207.842570099924,94.0508588661002,337.529582916972));
#24407=CARTESIAN_POINT('Ctrl Pts',(208.004370268359,94.0291299852868,338.176902674053));
#24408=CARTESIAN_POINT('Ctrl Pts',(208.057243536243,93.9929070890982,339.292622106622));
#24409=CARTESIAN_POINT('Ctrl Pts',(208.016331894512,93.978454139632,339.748263576678));
#24410=CARTESIAN_POINT('Ctrl Pts',(207.914727694784,93.9647376097703,340.191287620971));
#24411=CARTESIAN_POINT('Ctrl Pts',(207.914727694784,93.8397376070391,340.191287620971));
#24412=CARTESIAN_POINT('Ctrl Pts',(207.935967918546,93.8426050294909,340.098674029625));
#24413=CARTESIAN_POINT('Ctrl Pts',(207.954588856772,93.8455090974102,340.005364892963));
#24414=CARTESIAN_POINT('Ctrl Pts',(208.078884475172,93.8683852535681,339.274122305723));
#24415=CARTESIAN_POINT('Ctrl Pts',(208.062584791422,93.8894843264772,338.62179155748));
#24416=CARTESIAN_POINT('Ctrl Pts',(207.779834645017,93.9320720445258,337.34726825639));
#24417=CARTESIAN_POINT('Ctrl Pts',(207.511284980159,93.9524504634837,336.738401830215));
#24418=CARTESIAN_POINT('Ctrl Pts',(206.75007369525,93.9932226693162,335.65496881214));
#24419=CARTESIAN_POINT('Ctrl Pts',(206.262967114288,94.0149436030176,335.192503985698));
#24420=CARTESIAN_POINT('Ctrl Pts',(205.157177240321,94.0575202620966,334.498311406653));
#24421=CARTESIAN_POINT('Ctrl Pts',(204.554237298208,94.0773596066746,334.265145804384));
#24422=CARTESIAN_POINT('Ctrl Pts',(203.26880863012,94.1175076261342,334.034648111059));
#24423=CARTESIAN_POINT('Ctrl Pts',(202.596978886693,94.1392247945297,334.049121097658));
#24424=CARTESIAN_POINT('Ctrl Pts',(201.322527127607,94.181825940921,334.33476443115));
#24425=CARTESIAN_POINT('Ctrl Pts',(200.730071495465,94.201735081733,334.593760553116));
#24426=CARTESIAN_POINT('Ctrl Pts',(199.654655314064,94.2418345342463,335.335400052225));
#24427=CARTESIAN_POINT('Ctrl Pts',(199.187619668244,94.2635477724379,335.818967168767));
#24428=CARTESIAN_POINT('Ctrl Pts',(198.483717999202,94.3061716474694,336.9196265378));
#24429=CARTESIAN_POINT('Ctrl Pts',(198.245453322367,94.3261485581309,337.520872530092));
#24430=CARTESIAN_POINT('Ctrl Pts',(198.004245813119,94.3662019884901,338.805172568024));
#24431=CARTESIAN_POINT('Ctrl Pts',(198.013314859826,94.3879111915484,339.477667365453));
#24432=CARTESIAN_POINT('Ctrl Pts',(198.289069313759,94.4305561402753,340.755148662006));
#24433=CARTESIAN_POINT('Ctrl Pts',(198.543545720082,94.4505985666671,341.349871025278));
#24434=CARTESIAN_POINT('Ctrl Pts',(199.277301834465,94.4906084776871,342.431643005062));
#24435=CARTESIAN_POINT('Ctrl Pts',(199.757703001535,94.5123135926319,342.902701650533));
#24436=CARTESIAN_POINT('Ctrl Pts',(200.853785712487,94.5549780616054,343.615183736526));
#24437=CARTESIAN_POINT('Ctrl Pts',(201.453535775631,94.5750835715499,343.857957267027));
#24438=CARTESIAN_POINT('Ctrl Pts',(202.736805082043,94.6150524111144,344.108615782547));
#24439=CARTESIAN_POINT('Ctrl Pts',(203.409851783221,94.6367534297841,344.104320766872));
#24440=CARTESIAN_POINT('Ctrl Pts',(204.689975400976,94.679435964273,343.837304914196));
#24441=CARTESIAN_POINT('Ctrl Pts',(205.286697065872,94.6996019930009,343.586811426813));
#24442=CARTESIAN_POINT('Ctrl Pts',(206.374039189645,94.739532143181,342.860012590828));
#24443=CARTESIAN_POINT('Ctrl Pts',(206.848618578616,94.7612290955408,342.382421692139));
#24444=CARTESIAN_POINT('Ctrl Pts',(207.544595588626,94.8025025722738,341.326856142823));
#24445=CARTESIAN_POINT('Ctrl Pts',(207.781276655283,94.8217217654369,340.773173206348));
#24446=CARTESIAN_POINT('Ctrl Pts',(207.914727694784,94.8397376070391,340.191287620971));
#24447=CARTESIAN_POINT('Origin',(203.041252647846,100.739737607039,339.073593133701));
#24448=CARTESIAN_POINT('',(207.914727694784,95.9647376097703,340.191287620971));
#24449=CARTESIAN_POINT('',(207.914727694784,95.8397376070391,340.191287620971));
#24450=CARTESIAN_POINT('',(207.914727694784,100.739737607039,340.191287620971));
#24451=CARTESIAN_POINT('Ctrl Pts',(207.914727694784,95.9647376097703,340.191287620971));
#24452=CARTESIAN_POINT('Ctrl Pts',(207.824263172267,95.9525249322641,340.585739412711));
#24453=CARTESIAN_POINT('Ctrl Pts',(207.686054272076,95.9397175076353,340.968582041799));
#24454=CARTESIAN_POINT('Ctrl Pts',(207.20512380531,95.9053149036476,341.918957645222));
#24455=CARTESIAN_POINT('Ctrl Pts',(206.794450792268,95.8836127170631,342.44218957209));
#24456=CARTESIAN_POINT('Ctrl Pts',(205.807483630078,95.8424225905177,343.287698268786));
#24457=CARTESIAN_POINT('Ctrl Pts',(205.245149638245,95.8235684514315,343.607195840309));
#24458=CARTESIAN_POINT('Ctrl Pts',(204.014103711322,95.7816629611206,344.02200347778));
#24459=CARTESIAN_POINT('Ctrl Pts',(203.354969091086,95.7599713954899,344.106961722735));
#24460=CARTESIAN_POINT('Ctrl Pts',(202.058642119951,95.7187035695358,344.017842980232));
#24461=CARTESIAN_POINT('Ctrl Pts',(201.433368033154,95.6998747209822,343.851232320508));
#24462=CARTESIAN_POINT('Ctrl Pts',(200.2650806948,95.6580327952419,343.283741113733));
#24463=CARTESIAN_POINT('Ctrl Pts',(199.735999749879,95.6363534977267,342.882502476767));
#24464=CARTESIAN_POINT('Ctrl Pts',(198.87415919352,95.5950082285125,341.910306276557));
#24465=CARTESIAN_POINT('Ctrl Pts',(198.544931499865,95.5761962200961,341.352782574673));
#24466=CARTESIAN_POINT('Ctrl Pts',(198.109971183988,95.5344199939846,340.129152463659));
#24467=CARTESIAN_POINT('Ctrl Pts',(198.014078349114,95.5127546353721,339.472677632615));
#24468=CARTESIAN_POINT('Ctrl Pts',(198.080882444736,95.4713324948658,338.175326953219));
#24469=CARTESIAN_POINT('Ctrl Pts',(198.237066249138,95.4525284799068,337.546521770783));
#24470=CARTESIAN_POINT('Ctrl Pts',(198.784812691329,95.4108199169436,336.369203664002));
#24471=CARTESIAN_POINT('Ctrl Pts',(199.176290275722,95.389170170719,335.834291671704));
#24472=CARTESIAN_POINT('Ctrl Pts',(200.133192131337,95.3476720410362,334.955832806825));
#24473=CARTESIAN_POINT('Ctrl Pts',(200.68578868709,95.3288668896484,334.616626099003));
#24474=CARTESIAN_POINT('Ctrl Pts',(201.901705512363,95.2872277570585,334.16119097772));
#24475=CARTESIAN_POINT('Ctrl Pts',(202.555289211908,95.2655952775083,334.054220280177));
#24476=CARTESIAN_POINT('Ctrl Pts',(203.853482080545,95.2240223401788,334.098281489444));
#24477=CARTESIAN_POINT('Ctrl Pts',(204.485888896634,95.2052067610264,334.243844829991));
#24478=CARTESIAN_POINT('Ctrl Pts',(205.672192442344,95.1636386066622,334.771538039933));
#24479=CARTESIAN_POINT('Ctrl Pts',(206.212829695502,95.1420250074677,335.153054898725));
#24480=CARTESIAN_POINT('Ctrl Pts',(207.107967541355,95.1003787086922,336.094329255662));
#24481=CARTESIAN_POINT('Ctrl Pts',(207.457275026156,95.0815434134856,336.641941425247));
#24482=CARTESIAN_POINT('Ctrl Pts',(207.933233032709,95.0400475274432,337.849945808571));
#24483=CARTESIAN_POINT('Ctrl Pts',(208.051270303984,95.0184543591605,338.50044057598));
#24484=CARTESIAN_POINT('Ctrl Pts',(208.034882521879,94.986195370895,339.504782372743));
#24485=CARTESIAN_POINT('Ctrl Pts',(207.992537096821,94.9752418506327,339.852015857925));
#24486=CARTESIAN_POINT('Ctrl Pts',(207.914727694784,94.9647376097703,340.191287620971));
#24487=CARTESIAN_POINT('Ctrl Pts',(207.914727694784,94.8397376070391,340.191287620971));
#24488=CARTESIAN_POINT('Ctrl Pts',(207.924478876109,94.8410540129572,340.148769616808));
#24489=CARTESIAN_POINT('Ctrl Pts',(207.933678816981,94.842378252787,340.106101453216));
#24490=CARTESIAN_POINT('Ctrl Pts',(208.074323715298,94.8640459954571,339.409617319055));
#24491=CARTESIAN_POINT('Ctrl Pts',(208.074220596045,94.8857389434083,338.736113468209));
#24492=CARTESIAN_POINT('Ctrl Pts',(207.814880178946,94.9284536222466,337.453695970922));
#24493=CARTESIAN_POINT('Ctrl Pts',(207.567876777328,94.9487326644126,336.855221071499));
#24494=CARTESIAN_POINT('Ctrl Pts',(206.84718163009,94.9885922760571,335.763021977389));
#24495=CARTESIAN_POINT('Ctrl Pts',(206.372068480412,95.010281307781,335.285376670134));
#24496=CARTESIAN_POINT('Ctrl Pts',(205.283606284448,95.0530102443135,334.558772549594));
#24497=CARTESIAN_POINT('Ctrl Pts',(204.686316632632,95.0733417029364,334.308571751955));
#24498=CARTESIAN_POINT('Ctrl Pts',(203.404811224976,95.1131692964387,334.042386023179));
#24499=CARTESIAN_POINT('Ctrl Pts',(202.730929048368,95.1348545212918,334.038828048661));
#24500=CARTESIAN_POINT('Ctrl Pts',(201.446528139775,95.177596617987,334.291462750351));
#24501=CARTESIAN_POINT('Ctrl Pts',(200.846523620691,95.1979777630694,334.535423125413));
#24502=CARTESIAN_POINT('Ctrl Pts',(199.750108106285,95.2377753857359,335.250791257824));
#24503=CARTESIAN_POINT('Ctrl Pts',(199.269804452855,95.2594569296941,335.723732747906));
#24504=CARTESIAN_POINT('Ctrl Pts',(198.537473854873,95.3022111675649,336.8090732653));
#24505=CARTESIAN_POINT('Ctrl Pts',(198.284258664357,95.3226392971829,337.405365613395));
#24506=CARTESIAN_POINT('Ctrl Pts',(198.011786296759,95.3624089027797,338.686132005916));
#24507=CARTESIAN_POINT('Ctrl Pts',(198.005045724529,95.3840869044169,339.360327242861));
#24508=CARTESIAN_POINT('Ctrl Pts',(198.251849241647,95.4268523385324,340.6464372243));
#24509=CARTESIAN_POINT('Ctrl Pts',(198.493167953972,95.4473247985227,341.247770309472));
#24510=CARTESIAN_POINT('Ctrl Pts',(199.203908026909,95.4870682459829,342.347832116528));
#24511=CARTESIAN_POINT('Ctrl Pts',(199.674955959615,95.5087428529601,342.830432130254));
#24512=CARTESIAN_POINT('Ctrl Pts',(200.757578011136,95.5515186079928,343.567722277944));
#24513=CARTESIAN_POINT('Ctrl Pts',(201.353006720452,95.5720328081105,343.823549536321));
#24514=CARTESIAN_POINT('Ctrl Pts',(202.633122059699,95.6117518612847,344.101462174638));
#24515=CARTESIAN_POINT('Ctrl Pts',(203.307576481301,95.6334232273167,344.110958177241));
#24516=CARTESIAN_POINT('Ctrl Pts',(204.595154818141,95.6762084931767,343.869204754764));
#24517=CARTESIAN_POINT('Ctrl Pts',(205.197637349002,95.6967619200548,343.630170553606));
#24518=CARTESIAN_POINT('Ctrl Pts',(206.30084191883,95.7364582483519,342.923435407913));
#24519=CARTESIAN_POINT('Ctrl Pts',(206.785419220041,95.7581265306177,342.454031136491));
#24520=CARTESIAN_POINT('Ctrl Pts',(207.519374714258,95.8004811281553,341.38485900205));
#24521=CARTESIAN_POINT('Ctrl Pts',(207.774213604633,95.8207682561783,340.803970174115));
#24522=CARTESIAN_POINT('Ctrl Pts',(207.914727694784,95.8397376070391,340.191287620971));
#24523=CARTESIAN_POINT('Origin',(203.041252647846,100.739737607039,339.073593133701));
#24524=CARTESIAN_POINT('',(207.914727694784,96.9647376097703,340.191287620971));
#24525=CARTESIAN_POINT('',(207.914727695617,96.8397376072638,340.191287617342));
#24526=CARTESIAN_POINT('',(207.914727694784,100.739737607039,340.191287620971));
#24527=CARTESIAN_POINT('Ctrl Pts',(207.914727694784,96.9647376097703,340.191287620971));
#24528=CARTESIAN_POINT('Ctrl Pts',(207.802758576459,96.9496218196826,340.679505743544));
#24529=CARTESIAN_POINT('Ctrl Pts',(207.617885049872,96.9336271777375,341.148895869011));
#24530=CARTESIAN_POINT('Ctrl Pts',(207.033046171459,96.8957326294959,342.156559782157));
#24531=CARTESIAN_POINT('Ctrl Pts',(206.589773997112,96.873996568844,342.657882666583));
#24532=CARTESIAN_POINT('Ctrl Pts',(205.551746357524,96.8334013638026,343.44473295342));
#24533=CARTESIAN_POINT('Ctrl Pts',(204.972328379496,96.8141145725655,343.729815324878));
#24534=CARTESIAN_POINT('Ctrl Pts',(203.715974179417,96.7717892909509,344.071920067185));
#24535=CARTESIAN_POINT('Ctrl Pts',(203.048772405948,96.7500533743099,344.117252401768));
#24536=CARTESIAN_POINT('Ctrl Pts',(201.757683954315,96.7093888818263,343.948209884819));
#24537=CARTESIAN_POINT('Ctrl Pts',(201.145037418942,96.6901718243182,343.744119645876));
#24538=CARTESIAN_POINT('Ctrl Pts',(200.010917971376,96.6478900055346,343.10534129423));
#24539=CARTESIAN_POINT('Ctrl Pts',(199.504486762997,96.6261551884195,342.669318414581));
#24540=CARTESIAN_POINT('Ctrl Pts',(198.704275191607,96.5854194963093,341.64265857057));
#24541=CARTESIAN_POINT('Ctrl Pts',(198.411418202559,96.5662692169798,341.067111015307));
#24542=CARTESIAN_POINT('Ctrl Pts',(198.052703007714,96.5240334352275,339.816339987299));
#24543=CARTESIAN_POINT('Ctrl Pts',(197.998299814888,96.50230078477,339.150771078765));
#24544=CARTESIAN_POINT('Ctrl Pts',(198.149161486812,96.4614921819654,337.858277818631));
#24545=CARTESIAN_POINT('Ctrl Pts',(198.344699968257,96.4424049656356,337.242760738268));
#24546=CARTESIAN_POINT('Ctrl Pts',(198.967183994334,96.4002178223554,336.100610832859));
#24547=CARTESIAN_POINT('Ctrl Pts',(199.39532605161,96.378488515302,335.588782491954));
#24548=CARTESIAN_POINT('Ctrl Pts',(200.409639746461,96.3376055173355,334.774257765139));
#24549=CARTESIAN_POINT('Ctrl Pts',(200.981029093973,96.3185768779145,334.473032872092));
#24550=CARTESIAN_POINT('Ctrl Pts',(202.225700550231,96.2764409817612,334.096558489346));
#24551=CARTESIAN_POINT('Ctrl Pts',(202.889386226885,96.254716299989,334.032466287752));
#24552=CARTESIAN_POINT('Ctrl Pts',(204.183246902875,96.2137576725481,334.163838007811));
#24553=CARTESIAN_POINT('Ctrl Pts',(204.801842125211,96.1947823566162,334.350228466268));
#24554=CARTESIAN_POINT('Ctrl Pts',(205.952429364643,96.152700301268,334.955295933928));
#24555=CARTESIAN_POINT('Ctrl Pts',(206.469882603075,96.130981624657,335.374966376931));
#24556=CARTESIAN_POINT('Ctrl Pts',(207.299557325334,96.0899464045161,336.376016829161));
#24557=CARTESIAN_POINT('Ctrl Pts',(207.609688134916,96.0710184111409,336.942988721906));
#24558=CARTESIAN_POINT('Ctrl Pts',(208.004923802077,96.0289927512247,338.181070053893));
#24559=CARTESIAN_POINT('Ctrl Pts',(208.079237868111,96.0072815478085,338.842611471355));
#24560=CARTESIAN_POINT('Ctrl Pts',(208.003131952573,95.9790228405794,339.732835166694));
#24561=CARTESIAN_POINT('Ctrl Pts',(207.966858318546,95.9717752249422,339.963982845851));
#24562=CARTESIAN_POINT('Ctrl Pts',(207.914727694784,95.9647376097703,340.191287620971));
#24563=CARTESIAN_POINT('Ctrl Pts',(207.914727694784,95.8397376070391,340.191287620971));
#24564=CARTESIAN_POINT('Ctrl Pts',(207.917733844739,95.8401434361853,340.178179927447));
#24565=CARTESIAN_POINT('Ctrl Pts',(207.920687659849,95.8405500173302,340.16505772174));
#24566=CARTESIAN_POINT('Ctrl Pts',(208.067676524099,95.861185965235,339.499537617138));
#24567=CARTESIAN_POINT('Ctrl Pts',(208.079549757705,95.8828513221919,338.824868410798));
#24568=CARTESIAN_POINT('Ctrl Pts',(207.842154541268,95.9256534193295,337.536031690224));
#24569=CARTESIAN_POINT('Ctrl Pts',(207.605089455537,95.9462781151005,336.932558046077));
#24570=CARTESIAN_POINT('Ctrl Pts',(206.901808138952,95.9859336316715,335.826652492034));
#24571=CARTESIAN_POINT('Ctrl Pts',(206.433825071212,96.0075962212339,335.34037734793));
#24572=CARTESIAN_POINT('Ctrl Pts',(205.355596669194,96.0504057487236,334.595124501188));
#24573=CARTESIAN_POINT('Ctrl Pts',(204.761554490437,96.0710626810747,334.335100588781));
#24574=CARTESIAN_POINT('Ctrl Pts',(203.48250572603,96.1106999312182,334.048461908613));
#24575=CARTESIAN_POINT('Ctrl Pts',(202.807658305392,96.1323599092629,334.034543937213));
#24576=CARTESIAN_POINT('Ctrl Pts',(201.517745444591,96.1751762771804,334.268189510977));
#24577=CARTESIAN_POINT('Ctrl Pts',(200.913419707451,96.1958633175214,334.503562189406));
#24578=CARTESIAN_POINT('Ctrl Pts',(199.805198588,96.235483612383,335.20387374646));
#24579=CARTESIAN_POINT('Ctrl Pts',(199.317469007499,96.2571411315419,335.670632076405));
#24580=CARTESIAN_POINT('Ctrl Pts',(198.569056120019,96.2999637957029,336.74710683773));
#24581=CARTESIAN_POINT('Ctrl Pts',(198.307365685623,96.3206789206186,337.340598748464));
#24582=CARTESIAN_POINT('Ctrl Pts',(198.017266886641,96.3602834889125,338.619216989787));
#24583=CARTESIAN_POINT('Ctrl Pts',(198.00159474125,96.3819386976183,339.294212494069));
#24584=CARTESIAN_POINT('Ctrl Pts',(198.232022732549,96.4247671562484,340.585043979386));
#24585=CARTESIAN_POINT('Ctrl Pts',(198.465944416523,96.4455084479489,341.190100444113));
#24586=CARTESIAN_POINT('Ctrl Pts',(199.163708936799,96.4850984393755,342.300302492973));
#24587=CARTESIAN_POINT('Ctrl Pts',(199.629414875849,96.5067514811264,342.789275472743));
#24588=CARTESIAN_POINT('Ctrl Pts',(200.704383676333,96.5495852717304,343.540393904999));
#24589=CARTESIAN_POINT('Ctrl Pts',(201.297404439508,96.5703509173616,343.803511674489));
#24590=CARTESIAN_POINT('Ctrl Pts',(202.575650815693,96.6099274061719,344.096571660111));
#24591=CARTESIAN_POINT('Ctrl Pts',(203.250769555504,96.6315784189847,344.113745348026));
#24592=CARTESIAN_POINT('Ctrl Pts',(204.542310650037,96.6744146825828,343.88608507479));
#24593=CARTESIAN_POINT('Ctrl Pts',(205.14800052983,96.6951880189483,343.653432514059));
#24594=CARTESIAN_POINT('Ctrl Pts',(206.259678905628,96.7347749658355,342.957982630121));
#24595=CARTESIAN_POINT('Ctrl Pts',(206.749582166859,96.7563997669483,342.493414757975));
#24596=CARTESIAN_POINT('Ctrl Pts',(207.503033771944,96.7992350732268,341.420048159803));
#24597=CARTESIAN_POINT('Ctrl Pts',(207.767488036637,96.8200152451585,340.827475204036));
#24598=CARTESIAN_POINT('Ctrl Pts',(207.913228308978,96.8395355905515,340.197810353621));
#24599=CARTESIAN_POINT('Ctrl Pts',(207.913979658144,96.8396366223653,340.194549279651));
#24600=CARTESIAN_POINT('Ctrl Pts',(207.914727696449,96.8397376072639,340.191287613713));
#24601=CARTESIAN_POINT('Origin',(203.041252647846,100.739737607039,339.073593133701));
#24602=CARTESIAN_POINT('',(207.914727694784,97.9647376097703,340.191287620971));
#24603=CARTESIAN_POINT('',(207.914727694784,97.8397376070391,340.191287620971));
#24604=CARTESIAN_POINT('',(207.914727694784,100.739737607039,340.191287620971));
#24605=CARTESIAN_POINT('Ctrl Pts',(207.914727694784,97.9647376097703,340.191287620971));
#24606=CARTESIAN_POINT('Ctrl Pts',(207.787344310009,97.9475408993404,340.746716456103));
#24607=CARTESIAN_POINT('Ctrl Pts',(207.565819195648,97.9292362257558,341.276822047888));
#24608=CARTESIAN_POINT('Ctrl Pts',(206.901920889685,97.8889040001007,342.319839977017));
#24609=CARTESIAN_POINT('Ctrl Pts',(206.43604964038,97.8671886475898,342.804314532998));
#24610=CARTESIAN_POINT('Ctrl Pts',(205.362471371289,97.8270635922768,343.548222783882));
#24611=CARTESIAN_POINT('Ctrl Pts',(204.770668362569,97.807191468124,343.808521014367));
#24612=CARTESIAN_POINT('Ctrl Pts',(203.497095441832,97.7646031657314,344.097007748173));
#24613=CARTESIAN_POINT('Ctrl Pts',(202.825464906029,97.7428839628591,344.113034782473));
#24614=CARTESIAN_POINT('Ctrl Pts',(201.539719183794,97.7027089703224,343.88561945709));
#24615=CARTESIAN_POINT('Ctrl Pts',(200.936291916441,97.682907612388,343.653919449903));
#24616=CARTESIAN_POINT('Ctrl Pts',(199.829036312802,97.6403447783789,342.962518401829));
#24617=CARTESIAN_POINT('Ctrl Pts',(199.340920528111,97.6186219243762,342.501371361285));
#24618=CARTESIAN_POINT('Ctrl Pts',(198.58786600622,97.5783944155194,341.435242719625));
#24619=CARTESIAN_POINT('Ctrl Pts',(198.322311749214,97.5586653959233,340.846072140563));
#24620=CARTESIAN_POINT('Ctrl Pts',(198.022373280032,97.5161299491114,339.5760737029));
#24621=CARTESIAN_POINT('Ctrl Pts',(198.000086686688,97.4944037145157,338.90528166429));
#24622=CARTESIAN_POINT('Ctrl Pts',(198.21507454351,97.4541211107053,337.618292996073));
#24623=CARTESIAN_POINT('Ctrl Pts',(198.440874064337,97.4344656325874,337.012901703184));
#24624=CARTESIAN_POINT('Ctrl Pts',(199.121033095641,97.3919595955806,335.899785438682));
#24625=CARTESIAN_POINT('Ctrl Pts',(199.576857259965,97.3702303299924,335.407643650929));
#24626=CARTESIAN_POINT('Ctrl Pts',(200.634604874495,97.3298900735479,334.644393824861));
#24627=CARTESIAN_POINT('Ctrl Pts',(201.220838033555,97.3103089114501,334.37296716565));
#24628=CARTESIAN_POINT('Ctrl Pts',(202.486792604429,97.267834408313,334.060284171213));
#24629=CARTESIAN_POINT('Ctrl Pts',(203.156583106232,97.2461025479247,334.031030878434));
#24630=CARTESIAN_POINT('Ctrl Pts',(204.44489054434,97.2057021245588,334.232163093726));
#24631=CARTESIAN_POINT('Ctrl Pts',(205.052470447681,97.1861955643755,334.451399251097));
#24632=CARTESIAN_POINT('Ctrl Pts',(206.172029626128,97.1437548165742,335.119048848787));
#24633=CARTESIAN_POINT('Ctrl Pts',(206.668579130893,97.1220208912257,335.568920805684));
#24634=CARTESIAN_POINT('Ctrl Pts',(207.443095964537,97.0815578542201,336.617310321601));
#24635=CARTESIAN_POINT('Ctrl Pts',(207.721030489256,97.0621256342267,337.200292870474));
#24636=CARTESIAN_POINT('Ctrl Pts',(208.047773151692,97.0197209546451,338.461705833607));
#24637=CARTESIAN_POINT('Ctrl Pts',(208.084711340844,96.9979855941344,339.130307545868));
#24638=CARTESIAN_POINT('Ctrl Pts',(207.970544832191,96.9730848870396,339.922698137084));
#24639=CARTESIAN_POINT('Ctrl Pts',(207.945365996894,96.9688737693673,340.057695657771));
#24640=CARTESIAN_POINT('Ctrl Pts',(207.914727694784,96.9647376097703,340.191287620971));
#24641=CARTESIAN_POINT('Ctrl Pts',(207.914727696449,96.8397376072638,340.191287613713));
#24642=CARTESIAN_POINT('Ctrl Pts',(208.063328933394,96.8597987201314,339.543342729492));
#24643=CARTESIAN_POINT('Ctrl Pts',(208.08124770444,96.8813197613063,338.872133546454));
#24644=CARTESIAN_POINT('Ctrl Pts',(207.857183886755,96.9240413712455,337.583545012411));
#24645=CARTESIAN_POINT('Ctrl Pts',(207.625856930496,96.9448288876363,336.977191066835));
#24646=CARTESIAN_POINT('Ctrl Pts',(206.93304948772,96.9844430827078,335.864220560912));
#24647=CARTESIAN_POINT('Ctrl Pts',(206.469956438707,97.0060063639469,335.373555488612));
#24648=CARTESIAN_POINT('Ctrl Pts',(205.398715375365,97.0488325593009,334.617596147755));
#24649=CARTESIAN_POINT('Ctrl Pts',(204.806648547122,97.0696279611766,334.351625580777));
#24650=CARTESIAN_POINT('Ctrl Pts',(203.530305761832,97.1092573479852,334.052970476787));
#24651=CARTESIAN_POINT('Ctrl Pts',(202.856178857879,97.1307865267325,334.032590951377));
#24652=CARTESIAN_POINT('Ctrl Pts',(201.564004220546,97.1736075615292,334.253698191725));
#24653=CARTESIAN_POINT('Ctrl Pts',(200.956882423605,97.1944114231065,334.483482987031));
#24654=CARTESIAN_POINT('Ctrl Pts',(199.842414909669,97.2340571395576,335.173220322507));
#24655=CARTESIAN_POINT('Ctrl Pts',(199.350867401544,97.2555498199762,335.634602701572));
#24656=CARTESIAN_POINT('Ctrl Pts',(198.592002627439,97.298365242755,336.703373002197));
#24657=CARTESIAN_POINT('Ctrl Pts',(198.324273365712,97.3191781723567,337.294847654029));
#24658=CARTESIAN_POINT('Ctrl Pts',(198.022141535132,97.3588414296567,338.569990487973));
#24659=CARTESIAN_POINT('Ctrl Pts',(197.999789315069,97.380295088947,339.243486651965));
#24660=CARTESIAN_POINT('Ctrl Pts',(198.216804747761,97.4231044082145,340.535988376863));
#24661=CARTESIAN_POINT('Ctrl Pts',(198.444798541592,97.4439270490012,341.143995608951));
#24662=CARTESIAN_POINT('Ctrl Pts',(199.130975740103,97.4836091344146,342.260193371317));
#24663=CARTESIAN_POINT('Ctrl Pts',(199.590378227264,97.5050211231525,342.752760609713));
#24664=CARTESIAN_POINT('Ctrl Pts',(200.656281796591,97.5478238038946,343.514983608002));
#24665=CARTESIAN_POINT('Ctrl Pts',(201.247064215775,97.5686568343686,343.784748201602));
#24666=CARTESIAN_POINT('Ctrl Pts',(202.520812401028,97.6083591137349,344.090902697033));
#24667=CARTESIAN_POINT('Ctrl Pts',(203.193578172053,97.6297266576778,344.115534002417));
#24668=CARTESIAN_POINT('Ctrl Pts',(204.486448535759,97.672522117612,343.903250727198));
#24669=CARTESIAN_POINT('Ctrl Pts',(205.09547356045,97.693366251844,343.677332749677));
#24670=CARTESIAN_POINT('Ctrl Pts',(206.213665650385,97.7330901717824,342.995274731163));
#24671=CARTESIAN_POINT('Ctrl Pts',(206.707408045531,97.7544103753982,342.538157922658));
#24672=CARTESIAN_POINT('Ctrl Pts',(207.473501983227,97.7971979809594,341.475573328025));
#24673=CARTESIAN_POINT('Ctrl Pts',(207.745616027229,97.8180539684817,340.885599218779));
#24674=CARTESIAN_POINT('Ctrl Pts',(207.904004576751,97.8383099149618,340.237295052471));
#24675=CARTESIAN_POINT('Ctrl Pts',(207.909448526219,97.8390249212105,340.214306340814));
#24676=CARTESIAN_POINT('Ctrl Pts',(207.914727694784,97.8397376070391,340.191287620971));
#24677=CARTESIAN_POINT('Origin',(203.041252647846,100.739737607039,339.073593133701));
#24678=CARTESIAN_POINT('',(207.914727694784,98.9647376097703,340.191287620971));
#24679=CARTESIAN_POINT('',(207.914727694784,98.8397376070391,340.191287620971));
#24680=CARTESIAN_POINT('',(207.914727694784,100.739737607039,340.191287620971));
#24681=CARTESIAN_POINT('Ctrl Pts',(207.914727694784,98.9647376097703,340.191287620971));
#24682=CARTESIAN_POINT('Ctrl Pts',(207.777720932146,98.946241746843,340.788677199773));
#24683=CARTESIAN_POINT('Ctrl Pts',(207.531967934148,98.9264853686005,341.356088920239));
#24684=CARTESIAN_POINT('Ctrl Pts',(206.816955231582,98.8846656052097,342.418639843526));
#24685=CARTESIAN_POINT('Ctrl Pts',(206.337323742344,98.8629821131841,342.892132496792));
#24686=CARTESIAN_POINT('Ctrl Pts',(205.241974815253,98.8231687433469,343.608850647877));
#24687=CARTESIAN_POINT('Ctrl Pts',(204.642357902887,98.8028137788264,343.853581963425));
#24688=CARTESIAN_POINT('Ctrl Pts',(203.358458006767,98.7600785743928,344.107916703837));
#24689=CARTESIAN_POINT('Ctrl Pts',(202.684669887813,98.7383913324243,344.105286778262));
#24690=CARTESIAN_POINT('Ctrl Pts',(201.402951603227,98.6985469105573,343.84093487211));
#24691=CARTESIAN_POINT('Ctrl Pts',(200.80537116807,98.678243087483,343.591612575252));
#24692=CARTESIAN_POINT('Ctrl Pts',(199.716002334855,98.6355216189368,342.866677931433));
#24693=CARTESIAN_POINT('Ctrl Pts',(199.240259038187,98.6138305093857,342.389809004803));
#24694=CARTESIAN_POINT('Ctrl Pts',(198.518014230854,98.5739529391946,341.298840423343));
#24695=CARTESIAN_POINT('Ctrl Pts',(198.270125087002,98.5537029931734,340.700810587759));
#24696=CARTESIAN_POINT('Ctrl Pts',(198.008835158704,98.5109964017973,339.418973330549));
#24697=CARTESIAN_POINT('Ctrl Pts',(198.007667454863,98.4893013260074,338.745583151298));
#24698=CARTESIAN_POINT('Ctrl Pts',(198.264512112369,98.4493884220293,337.463006106893));
#24699=CARTESIAN_POINT('Ctrl Pts',(198.510241726302,98.4291950789849,336.864235846117));
#24700=CARTESIAN_POINT('Ctrl Pts',(199.228346402579,98.3865045914073,335.771173993807));
#24701=CARTESIAN_POINT('Ctrl Pts',(199.702032695211,98.3648054745532,335.292866694799));
#24702=CARTESIAN_POINT('Ctrl Pts',(200.787961132659,98.3248549668108,334.564297820753));
#24703=CARTESIAN_POINT('Ctrl Pts',(201.384174238201,98.304720913041,334.312791512603));
#24704=CARTESIAN_POINT('Ctrl Pts',(202.663628399212,98.2620478454922,334.043551398921));
#24705=CARTESIAN_POINT('Ctrl Pts',(203.336537802058,98.2403446419795,334.038041373913));
#24706=CARTESIAN_POINT('Ctrl Pts',(204.6200724226,98.2003541822505,334.286295452556));
#24707=CARTESIAN_POINT('Ctrl Pts',(205.220203173367,98.1802820300518,334.527921049304));
#24708=CARTESIAN_POINT('Ctrl Pts',(206.317454637024,98.1376277923591,335.238219079962));
#24709=CARTESIAN_POINT('Ctrl Pts',(206.798665037818,98.1159204917686,335.708255199108));
#24710=CARTESIAN_POINT('Ctrl Pts',(207.534431521013,98.0758876616242,336.788410847114));
#24711=CARTESIAN_POINT('Ctrl Pts',(207.790059825899,98.0558799103887,337.382555301657));
#24712=CARTESIAN_POINT('Ctrl Pts',(208.068337373195,98.0132460095855,338.659267602543));
#24713=CARTESIAN_POINT('Ctrl Pts',(208.078785073144,97.9915346431374,339.331596807135));
#24714=CARTESIAN_POINT('Ctrl Pts',(207.944503674349,97.9689676904175,340.05492519118));
#24715=CARTESIAN_POINT('Ctrl Pts',(207.930321147104,97.9668427201395,340.123295605584));
#24716=CARTESIAN_POINT('Ctrl Pts',(207.914727694784,97.9647376097703,340.191287620971));
#24717=CARTESIAN_POINT('Ctrl Pts',(207.914727694784,97.8397376070391,340.191287620971));
#24718=CARTESIAN_POINT('Ctrl Pts',(208.058182547195,97.8591039597311,339.56578248379));
#24719=CARTESIAN_POINT('Ctrl Pts',(208.07993750736,97.8798428986119,338.918208288944));
#24720=CARTESIAN_POINT('Ctrl Pts',(207.876844768975,97.921849972268,337.648264029656));
#24721=CARTESIAN_POINT('Ctrl Pts',(207.653327094259,97.9427185975742,337.038073358269));
#24722=CARTESIAN_POINT('Ctrl Pts',(206.976022784969,97.982490470181,335.91758985581));
#24723=CARTESIAN_POINT('Ctrl Pts',(206.521536947544,98.0037068514112,335.42249745158));
#24724=CARTESIAN_POINT('Ctrl Pts',(205.462785275897,98.0464766207395,334.651955691748));
#24725=CARTESIAN_POINT('Ctrl Pts',(204.873753760568,98.0673587023253,334.377137639582));
#24726=CARTESIAN_POINT('Ctrl Pts',(203.603496057517,98.10715705557,334.060999305767));
#24727=CARTESIAN_POINT('Ctrl Pts',(202.932545649898,98.1283167494464,334.030727003283));
#24728=CARTESIAN_POINT('Ctrl Pts',(201.638805561778,98.1710764119139,334.231275804564));
#24729=CARTESIAN_POINT('Ctrl Pts',(201.027285562879,98.1919728007889,334.452025495068));
#24730=CARTESIAN_POINT('Ctrl Pts',(199.904178929685,98.2317994170826,335.123860172382));
#24731=CARTESIAN_POINT('Ctrl Pts',(199.407541238451,98.2528991230827,335.57532779236));
#24732=CARTESIAN_POINT('Ctrl Pts',(198.631907392309,98.295647794643,336.629665876014));
#24733=CARTESIAN_POINT('Ctrl Pts',(198.353987917779,98.316559372242,337.217599990389));
#24734=CARTESIAN_POINT('Ctrl Pts',(198.031724659258,98.3564161178684,338.485695774884));
#24735=CARTESIAN_POINT('Ctrl Pts',(197.998002447511,98.3774524682769,339.155530828702));
#24736=CARTESIAN_POINT('Ctrl Pts',(198.191359714666,98.4201891897461,340.449772811658));
#24737=CARTESIAN_POINT('Ctrl Pts',(198.408927445719,98.4411168651635,341.062801411641));
#24738=CARTESIAN_POINT('Ctrl Pts',(199.074490349552,98.4810056885441,342.188898326382));
#24739=CARTESIAN_POINT('Ctrl Pts',(199.522508907796,98.5019752688356,342.687297558801));
#24740=CARTESIAN_POINT('Ctrl Pts',(200.571781851861,98.5446990005184,343.468736769743));
#24741=CARTESIAN_POINT('Ctrl Pts',(201.158440861306,98.5656437069934,343.75019947828));
#24742=CARTESIAN_POINT('Ctrl Pts',(202.424048234059,98.6055666358783,344.07945836568));
#24743=CARTESIAN_POINT('Ctrl Pts',(203.092608024152,98.6264660090367,344.117111082783));
#24744=CARTESIAN_POINT('Ctrl Pts',(204.387394029372,98.6691756252586,343.931960667624));
#24745=CARTESIAN_POINT('Ctrl Pts',(205.002125100582,98.690138315837,343.718037509402));
#24746=CARTESIAN_POINT('Ctrl Pts',(206.131614507215,98.7300974532906,343.059637825064));
#24747=CARTESIAN_POINT('Ctrl Pts',(206.632012430995,98.7509231883392,342.615543230054));
#24748=CARTESIAN_POINT('Ctrl Pts',(207.42003869431,98.7936174719612,341.572060645236));
#24749=CARTESIAN_POINT('Ctrl Pts',(207.705531099556,98.8145991142706,340.986879656359));
#24750=CARTESIAN_POINT('Ctrl Pts',(207.887254109002,98.8361536439949,340.306386204824));
#24751=CARTESIAN_POINT('Ctrl Pts',(207.901506963965,98.8379528132061,340.248933876262));
#24752=CARTESIAN_POINT('Ctrl Pts',(207.914727694784,98.8397376070391,340.191287620971));
#24753=CARTESIAN_POINT('Origin',(203.041252647846,100.739737607039,339.073593133701));
#24754=CARTESIAN_POINT('',(207.914727692943,99.9647376092732,340.191287628998));
#24755=CARTESIAN_POINT('',(207.914727694784,99.8397376070391,340.191287620971));
#24756=CARTESIAN_POINT('',(207.914727694784,100.739737607039,340.191287620971));
#24757=CARTESIAN_POINT('Ctrl Pts',(207.914727691102,99.9647376092732,340.191287637025));
#24758=CARTESIAN_POINT('Ctrl Pts',(207.772226000692,99.9454999333533,340.812636699557));
#24759=CARTESIAN_POINT('Ctrl Pts',(207.512177670137,99.9249116561356,341.401134030297));
#24760=CARTESIAN_POINT('Ctrl Pts',(206.767415734281,99.8822557941594,342.473938918684));
#24761=CARTESIAN_POINT('Ctrl Pts',(206.280052374215,99.8605969813808,342.94100626745));
#24762=CARTESIAN_POINT('Ctrl Pts',(205.172414462498,99.8209677950671,343.642066565408));
#24763=CARTESIAN_POINT('Ctrl Pts',(204.568303547233,99.8002965657112,343.877865874889));
#24764=CARTESIAN_POINT('Ctrl Pts',(203.278661492023,99.7574837781782,344.112457012639));
#24765=CARTESIAN_POINT('Ctrl Pts',(202.603858439339,99.735822425517,344.099054622666));
#24766=CARTESIAN_POINT('Ctrl Pts',(201.324683937858,99.6961755945932,343.813433082381));
#24767=CARTESIAN_POINT('Ctrl Pts',(200.730480054175,99.6755355963093,343.553898797219));
#24768=CARTESIAN_POINT('Ctrl Pts',(199.651737388951,99.632729958152,342.809574598577));
#24769=CARTESIAN_POINT('Ctrl Pts',(199.183395314978,99.6110659111106,342.323727313663));
#24770=CARTESIAN_POINT('Ctrl Pts',(198.479242320269,99.5714000791075,341.218502623156));
#24771=CARTESIAN_POINT('Ctrl Pts',(198.241680356331,99.5507934959721,340.615279102861));
#24772=CARTESIAN_POINT('Ctrl Pts',(198.003184949077,99.5079956229591,339.326759280724));
#24773=CARTESIAN_POINT('Ctrl Pts',(198.014458134513,99.4863287244055,338.652143518686));
#24774=CARTESIAN_POINT('Ctrl Pts',(198.295878414244,99.4466424476291,337.372453614684));
#24775=CARTESIAN_POINT('Ctrl Pts',(198.553391574092,99.4260715654506,336.777582057841));
#24776=CARTESIAN_POINT('Ctrl Pts',(199.293881381493,99.3832821245836,335.696721190546));
#24777=CARTESIAN_POINT('Ctrl Pts',(199.777959926478,99.3616122161077,335.226901158811));
#24778=CARTESIAN_POINT('Ctrl Pts',(200.880371479858,99.3219039609348,334.519154046494));
#24779=CARTESIAN_POINT('Ctrl Pts',(201.482563588122,99.3013711628205,334.279542718545));
#24780=CARTESIAN_POINT('Ctrl Pts',(202.76977183055,99.2585908761615,334.036512880947));
#24781=CARTESIAN_POINT('Ctrl Pts',(203.44416178828,99.2369177997395,334.045312525477));
#24782=CARTESIAN_POINT('Ctrl Pts',(204.724442646349,99.1971859403622,334.321850504282));
#24783=CARTESIAN_POINT('Ctrl Pts',(205.320089637049,99.1766937002196,334.577017428622));
#24784=CARTESIAN_POINT('Ctrl Pts',(206.403400096601,99.1339233488994,335.31305403556));
#24785=CARTESIAN_POINT('Ctrl Pts',(206.874927747583,99.1122469489044,335.79507416393));
#24786=CARTESIAN_POINT('Ctrl Pts',(207.586838848766,99.0724897656359,336.894214834667));
#24787=CARTESIAN_POINT('Ctrl Pts',(207.828825798982,99.0520406392946,337.49521178462));
#24788=CARTESIAN_POINT('Ctrl Pts',(208.077105239224,99.0092810676856,338.780890563379));
#24789=CARTESIAN_POINT('Ctrl Pts',(208.071170113211,98.9876011932843,339.455007960196));
#24790=CARTESIAN_POINT('Ctrl Pts',(207.927190449723,98.966454936529,340.135864050133));
#24791=CARTESIAN_POINT('Ctrl Pts',(207.921075822522,98.9655946046969,340.163607926315));
#24792=CARTESIAN_POINT('Ctrl Pts',(207.914727694784,98.9647376097703,340.191287620971));
#24793=CARTESIAN_POINT('Ctrl Pts',(207.914727694784,98.8397376070391,340.191287620971));
#24794=CARTESIAN_POINT('Ctrl Pts',(208.049234382686,98.8578959607898,339.604799099645));
#24795=CARTESIAN_POINT('Ctrl Pts',(208.076885361511,98.8772793791297,338.99831557964));
#24796=CARTESIAN_POINT('Ctrl Pts',(207.909025166348,98.9180229753005,337.761651286256));
#24797=CARTESIAN_POINT('Ctrl Pts',(207.699259005141,98.9390245453775,337.145011250203));
#24798=CARTESIAN_POINT('Ctrl Pts',(207.049003838244,98.9790626822083,336.011694015816));
#24799=CARTESIAN_POINT('Ctrl Pts',(206.609350999,98.999731041669,335.509040267232));
#24800=CARTESIAN_POINT('Ctrl Pts',(205.572458381145,99.0423906159896,334.713580437515));
#24801=CARTESIAN_POINT('Ctrl Pts',(204.98898562304,99.0634130911169,334.423528734006));
#24802=CARTESIAN_POINT('Ctrl Pts',(203.729493197537,99.1034941366792,334.077317783523));
#24803=CARTESIAN_POINT('Ctrl Pts',(203.064028612122,99.1240789539438,334.030183023473));
#24804=CARTESIAN_POINT('Ctrl Pts',(201.768052178728,99.1667189425487,334.195478139589));
#24805=CARTESIAN_POINT('Ctrl Pts',(201.149287222279,99.1877632930759,334.400525569592));
#24806=CARTESIAN_POINT('Ctrl Pts',(200.011677601723,99.2278895830345,335.041567981417));
#24807=CARTESIAN_POINT('Ctrl Pts',(199.506492864002,99.2483878268878,335.476221651959));
#24808=CARTESIAN_POINT('Ctrl Pts',(198.702695460361,99.2910065954628,336.505652435701));
#24809=CARTESIAN_POINT('Ctrl Pts',(198.40751551838,99.3120737756058,337.087157847669));
#24810=CARTESIAN_POINT('Ctrl Pts',(198.051185060294,99.3522476785371,338.342942483846));
#24811=CARTESIAN_POINT('Ctrl Pts',(197.998417906508,99.3726565343252,339.006556835035));
#24812=CARTESIAN_POINT('Ctrl Pts',(198.1518825264,99.4152523336181,340.303158655062));
#24813=CARTESIAN_POINT('Ctrl Pts',(198.351602925608,99.4363432712621,340.92426942185));
#24814=CARTESIAN_POINT('Ctrl Pts',(198.982284772655,99.476567175061,342.066658951876));
#24815=CARTESIAN_POINT('Ctrl Pts',(199.411348093172,99.4968840997243,342.57466469062));
#24816=CARTESIAN_POINT('Ctrl Pts',(200.432378756558,99.5394550628214,343.387749359463));
#24817=CARTESIAN_POINT('Ctrl Pts',(201.011627979659,99.5605706483865,343.688659209056));
#24818=CARTESIAN_POINT('Ctrl Pts',(202.263218809242,99.6008469448783,344.056296410767));
#24819=CARTESIAN_POINT('Ctrl Pts',(202.924764336384,99.621069725327,344.115332894066));
#24820=CARTESIAN_POINT('Ctrl Pts',(204.221990579288,99.6636138660953,343.975066633394));
#24821=CARTESIAN_POINT('Ctrl Pts',(204.845666986157,99.6847549405606,343.781322539685));
#24822=CARTESIAN_POINT('Ctrl Pts',(205.993337998062,99.7250860083536,343.162215832264));
#24823=CARTESIAN_POINT('Ctrl Pts',(206.504465036478,99.7452128223663,342.739358964637));
#24824=CARTESIAN_POINT('Ctrl Pts',(207.327815493964,99.78772803532,341.727722708046));
#24825=CARTESIAN_POINT('Ctrl Pts',(207.635079777938,99.8088953775479,341.151047887576));
#24826=CARTESIAN_POINT('Ctrl Pts',(207.858203404946,99.8325988852204,340.419266196908));
#24827=CARTESIAN_POINT('Ctrl Pts',(207.88849335847,99.8361959812164,340.305677004524));
#24828=CARTESIAN_POINT('Ctrl Pts',(207.914727694784,99.8397376070391,340.191287620971));
#24829=CARTESIAN_POINT('Origin',(203.041252647846,100.739737607039,339.073593133701));
#24830=CARTESIAN_POINT('',(204.158947135117,100.089737607039,334.200118086763));
#24831=CARTESIAN_POINT('Ctrl Pts',(207.914727694784,99.8397376070391,340.191287620971));
#24832=CARTESIAN_POINT('Ctrl Pts',(208.034767752977,99.8559429710617,339.667877838696));
#24833=CARTESIAN_POINT('Ctrl Pts',(208.069878022306,99.8731477517474,339.127777149765));
#24834=CARTESIAN_POINT('Ctrl Pts',(207.955567219792,99.9117971036651,337.94709393426));
#24835=CARTESIAN_POINT('Ctrl Pts',(207.768480675938,99.9329914172117,337.320640552275));
#24836=CARTESIAN_POINT('Ctrl Pts',(207.16221135957,99.9734390149761,336.167184155024));
#24837=CARTESIAN_POINT('Ctrl Pts',(206.746189859031,99.9933703048699,335.652631237103));
#24838=CARTESIAN_POINT('Ctrl Pts',(205.939101240561,100.027590364906,334.979846171942));
#24839=CARTESIAN_POINT('Ctrl Pts',(205.606479924445,100.040537817989,334.763616001554));
#24840=CARTESIAN_POINT('Ctrl Pts',(204.903851201034,100.065797691061,334.417277154942));
#24841=CARTESIAN_POINT('Ctrl Pts',(204.537074450298,100.078030353952,334.286838714568));
#24842=CARTESIAN_POINT('Ctrl Pts',(204.158947135116,100.089737607039,334.200118086763));
#24843=CARTESIAN_POINT('',(207.277649300794,100.089737607039,336.417855307993));
#24844=CARTESIAN_POINT('Origin',(203.041252647846,100.089737607039,339.073593133701));
#24845=CARTESIAN_POINT('Ctrl Pts',(207.277649300794,100.089737607039,336.417855307994));
#24846=CARTESIAN_POINT('Ctrl Pts',(207.62501622021,100.070001614885,336.971970266372));
#24847=CARTESIAN_POINT('Ctrl Pts',(207.860302304862,100.048852917176,337.588869716441));
#24848=CARTESIAN_POINT('Ctrl Pts',(208.080080674944,100.006125505448,338.878361907358));
#24849=CARTESIAN_POINT('Ctrl Pts',(208.062383836499,99.9849574354711,339.538574593748));
#24850=CARTESIAN_POINT('Ctrl Pts',(207.916957879617,99.9650397665077,340.181529749979));
#24851=CARTESIAN_POINT('Ctrl Pts',(207.91584640822,99.9648886356732,340.186409703085));
#24852=CARTESIAN_POINT('Ctrl Pts',(207.914727691102,99.9647376092732,340.191287637025));
#24853=CARTESIAN_POINT('Origin',(203.041252647846,100.739737607039,339.073593133701));
#24854=CARTESIAN_POINT('',(212.788202741722,85.7397376070391,341.308982108241));
#24855=CARTESIAN_POINT('Origin',(203.041252647846,85.7397376070391,339.073593133701));
#24856=CARTESIAN_POINT('',(212.788202741722,70.2397376070391,341.308982108241));
#24857=CARTESIAN_POINT('',(212.788202741722,100.739737607039,341.308982108241));
#24858=CARTESIAN_POINT('',(205.276641622387,70.2397376070391,329.326643039825));
#24859=CARTESIAN_POINT('Origin',(203.041252647846,70.2397376070391,339.073593133701));
#24860=CARTESIAN_POINT('',(193.294302553971,70.2397376070391,336.83820415916));
#24861=CARTESIAN_POINT('Origin',(203.041252647846,70.2397376070391,339.073593133701));
#24862=CARTESIAN_POINT('',(200.805863673306,70.2397376070391,348.820543227576));
#24863=CARTESIAN_POINT('Origin',(203.041252647846,70.2397376070391,339.073593133701));
#24864=CARTESIAN_POINT('Origin',(203.041252647846,70.2397376070391,339.073593133701));
#24865=CARTESIAN_POINT('Origin',(216.141286203533,40.2397376070391,326.688556967428));
#24866=CARTESIAN_POINT('',(210.105735972273,35.2397376070391,353.005322220892));
#24867=CARTESIAN_POINT('Origin',(210.105735972273,40.2397376070391,353.005322220892));
#24868=CARTESIAN_POINT('',(209.435119279911,35.2397376070391,355.929407249055));
#24869=CARTESIAN_POINT('',(216.141286203533,35.2397376070391,326.688556967428));
#24870=CARTESIAN_POINT('Origin',(209.435119279911,40.2397376070391,355.929407249055));
#24871=CARTESIAN_POINT('Origin',(216.141286203533,40.2397376070391,326.688556967428));
#24872=CARTESIAN_POINT('',(216.141286203533,35.2397376070391,326.688556967428));
#24873=CARTESIAN_POINT('Origin',(216.141286203533,40.2397376070391,326.688556967428));
#24874=CARTESIAN_POINT('',(215.470669511171,35.2397376070391,329.612641995591));
#24875=CARTESIAN_POINT('',(216.141286203533,35.2397376070391,326.688556967428));
#24876=CARTESIAN_POINT('Origin',(215.470669511171,40.2397376070391,329.612641995591));
#24877=CARTESIAN_POINT('Origin',(203.041252647846,100.739737607039,339.073593133701));
#24878=CARTESIAN_POINT('',(198.322260569661,100.248231256093,337.991328141994));
#24879=CARTESIAN_POINT('Ctrl Pts',(204.158947135117,100.089737607039,334.200118086763));
#24880=CARTESIAN_POINT('Ctrl Pts',(203.567986347669,100.101286651919,334.076434599289));
#24881=CARTESIAN_POINT('Ctrl Pts',(203.076964148285,100.11133952839,334.083193431931));
#24882=CARTESIAN_POINT('Ctrl Pts',(202.269604552341,100.128117897055,334.15059440257));
#24883=CARTESIAN_POINT('Ctrl Pts',(201.816482456597,100.137815372571,334.253306792782));
#24884=CARTESIAN_POINT('Ctrl Pts',(200.812021118434,100.159974179144,334.634292946593));
#24885=CARTESIAN_POINT('Ctrl Pts',(200.244344607109,100.17228394124,334.970269554068));
#24886=CARTESIAN_POINT('Ctrl Pts',(199.282907777807,100.199611537441,335.881659458326));
#24887=CARTESIAN_POINT('Ctrl Pts',(198.91269334307,100.213147705628,336.402192829191));
#24888=CARTESIAN_POINT('Ctrl Pts',(198.510734686059,100.233619853094,337.29194862115));
#24889=CARTESIAN_POINT('Ctrl Pts',(198.397399007679,100.240963808763,337.631191678964));
#24890=CARTESIAN_POINT('Ctrl Pts',(198.322260569661,100.248231256093,337.991328141994));
#24891=CARTESIAN_POINT('',(198.801329357011,100.739737607039,338.101198929776));
#24892=CARTESIAN_POINT('',(198.801329357011,100.739737607039,338.101198929776));
#24893=CARTESIAN_POINT('Origin',(203.041252647846,100.739737607039,339.073593133701));
#24894=CARTESIAN_POINT('',(207.107563775619,100.631003482039,337.244543159099));
#24895=CARTESIAN_POINT('Ctrl Pts',(198.322260569661,100.248231256093,337.991328141994));
#24896=CARTESIAN_POINT('Ctrl Pts',(198.265865587261,100.253685822026,338.261627738713));
#24897=CARTESIAN_POINT('Ctrl Pts',(198.231285693129,100.259483012085,338.543751260379));
#24898=CARTESIAN_POINT('Ctrl Pts',(198.205299560629,100.278651810169,339.458060951051));
#24899=CARTESIAN_POINT('Ctrl Pts',(198.308913933128,100.292192634244,340.07813647236));
#24900=CARTESIAN_POINT('Ctrl Pts',(198.735959685609,100.318070364889,341.214213314114));
#24901=CARTESIAN_POINT('Ctrl Pts',(199.058786882686,100.33037409878,341.76423347003));
#24902=CARTESIAN_POINT('Ctrl Pts',(199.726641142822,100.351123698728,342.473696291465));
#24903=CARTESIAN_POINT('Ctrl Pts',(199.956597002958,100.357752877431,342.674907245237));
#24904=CARTESIAN_POINT('Ctrl Pts',(200.684813343231,100.377376238089,343.197053078148));
#24905=CARTESIAN_POINT('Ctrl Pts',(201.22575207331,100.390328845839,343.448271766013));
#24906=CARTESIAN_POINT('Ctrl Pts',(202.379327369579,100.415014798707,343.739752840505));
#24907=CARTESIAN_POINT('Ctrl Pts',(202.976464577814,100.427516491142,343.773223792695));
#24908=CARTESIAN_POINT('Ctrl Pts',(204.172185811973,100.454347635149,343.610258087121));
#24909=CARTESIAN_POINT('Ctrl Pts',(204.755653114925,100.468015172787,343.408876554908));
#24910=CARTESIAN_POINT('Ctrl Pts',(205.542558502781,100.487313364515,342.948631399366));
#24911=CARTESIAN_POINT('Ctrl Pts',(205.786240387277,100.493517003125,342.772350110457));
#24912=CARTESIAN_POINT('Ctrl Pts',(206.443763515596,100.512731222331,342.189020750292));
#24913=CARTESIAN_POINT('Ctrl Pts',(206.799360258044,100.525914732775,341.726717280771));
#24914=CARTESIAN_POINT('Ctrl Pts',(207.328428666458,100.552463745409,340.675326282134));
#24915=CARTESIAN_POINT('Ctrl Pts',(207.491421017174,100.564937188876,340.089059350026));
#24916=CARTESIAN_POINT('Ctrl Pts',(207.560618501709,100.586849760216,339.103391640685));
#24917=CARTESIAN_POINT('Ctrl Pts',(207.537661983056,100.595710021862,338.715638501893));
#24918=CARTESIAN_POINT('Ctrl Pts',(207.393266348567,100.613507459,337.958136842933));
#24919=CARTESIAN_POINT('Ctrl Pts',(207.273057797548,100.622370230913,337.591420948307));
#24920=CARTESIAN_POINT('Ctrl Pts',(207.107563775619,100.631003482039,337.244543159099));
#24921=CARTESIAN_POINT('',(201.212202673244,100.631003482039,335.007282005928));
#24922=CARTESIAN_POINT('Origin',(203.041252647846,100.631003482039,339.073593133701));
#24923=CARTESIAN_POINT('Ctrl Pts',(201.212202673245,100.631003482039,335.007282005928));
#24924=CARTESIAN_POINT('Ctrl Pts',(201.692997247517,100.585063473448,334.740644369554));
#24925=CARTESIAN_POINT('Ctrl Pts',(202.2181597904,100.538067764303,334.563560685677));
#24926=CARTESIAN_POINT('Ctrl Pts',(203.34458799318,100.443271815276,334.400105891955));
#24927=CARTESIAN_POINT('Ctrl Pts',(203.930685093604,100.399102406969,334.431026796414));
#24928=CARTESIAN_POINT('Ctrl Pts',(205.043083613764,100.310330549729,334.698222656967));
#24929=CARTESIAN_POINT('Ctrl Pts',(205.558128812846,100.265685149075,334.920866681284));
#24930=CARTESIAN_POINT('Ctrl Pts',(206.260185161977,100.199312659861,335.381164329575));
#24931=CARTESIAN_POINT('Ctrl Pts',(206.482421957023,100.177253987256,335.556461106809));
#24932=CARTESIAN_POINT('Ctrl Pts',(206.970346125787,100.126107413338,336.015937249671));
#24933=CARTESIAN_POINT('Ctrl Pts',(207.163692240569,100.103490234527,336.261964855603));
#24934=CARTESIAN_POINT('Ctrl Pts',(207.277649300794,100.089737607039,336.417855307993));
#24935=CARTESIAN_POINT('Origin',(225.888236297409,70.2397376070391,328.923945941969));
#24936=CARTESIAN_POINT('',(220.299763861057,70.2397376070391,353.291321176658));
#24937=CARTESIAN_POINT('',(224.770541810138,70.2397376070391,333.797420988906));
#24938=CARTESIAN_POINT('',(225.888236297409,70.2397376070391,328.923945941969));
#24939=CARTESIAN_POINT('',(224.770541810138,70.2397376070391,333.797420988906));
#24940=CARTESIAN_POINT('',(220.299763861057,70.2397376070391,353.291321176658));
#24941=CARTESIAN_POINT('Origin',(225.888236297409,70.2397376070391,328.923945941969));
#24942=CARTESIAN_POINT('',(191.05891357943,70.2397376070391,346.585154253036));
#24943=CARTESIAN_POINT('',(196.647386015782,70.2397376070391,322.217779018347));
#24944=CARTESIAN_POINT('',(220.299763861057,70.2397376070391,353.291321176658));
#24945=CARTESIAN_POINT('Origin',(225.217619605046,31.2397376070391,331.848030970131));
#24946=CARTESIAN_POINT('',(225.145860085501,65.2397376070391,331.831573469348));
#24947=CARTESIAN_POINT('',(224.236987121615,39.9086604301851,331.623130358101));
#24948=CARTESIAN_POINT('',(223.927696189104,31.2884540946096,331.552196831839));
#24949=CARTESIAN_POINT('',(196.724771172371,65.2397376070391,325.313412589385));
#24950=CARTESIAN_POINT('',(195.97676932342,65.2397376070391,325.14186404651));
#24951=CARTESIAN_POINT('',(207.280643844697,37.0155488911437,327.734321813409));
#24952=CARTESIAN_POINT('',(211.465570642183,25.8259327067678,328.694102989291));
#24953=CARTESIAN_POINT('Origin',(215.470669511171,40.2397376070391,329.612641995591));
#24954=CARTESIAN_POINT('Origin',(225.888236297409,31.2397376070391,328.923945941969));
#24955=CARTESIAN_POINT('',(207.951260537059,37.0155488911437,324.810236785247));
#24956=CARTESIAN_POINT('',(197.395387864733,65.2397376070391,322.389327561222));
#24957=CARTESIAN_POINT('',(207.951260537059,37.0155488911437,324.810236785247));
#24958=CARTESIAN_POINT('',(225.816476777863,65.2397376070391,328.907488441185));
#24959=CARTESIAN_POINT('',(225.888236297409,65.2397376070391,328.923945941969));
#24960=CARTESIAN_POINT('',(224.907603813977,39.9086604301851,328.699045329938));
#24961=CARTESIAN_POINT('',(225.888236297409,67.2397376070391,328.923945941969));
#24962=CARTESIAN_POINT('Origin',(216.141286203533,40.2397376070391,326.688556967428));
#24963=CARTESIAN_POINT('Origin',(225.888236297409,70.2397376070391,328.923945941969));
#24964=CARTESIAN_POINT('',(195.529691528511,70.2397376070391,327.091254065285));
#24965=CARTESIAN_POINT('',(224.770541810138,70.2397376070391,333.797420988906));
#24966=CARTESIAN_POINT('',(196.647386015782,70.2397376070391,322.217779018347));
#24967=CARTESIAN_POINT('Origin',(219.182069373787,31.2397376070391,358.164796223596));
#24968=CARTESIAN_POINT('',(219.110309854242,65.2397376070391,358.148338722812));
#24969=CARTESIAN_POINT('',(218.201436890355,39.9086604301851,357.939895611565));
#24970=CARTESIAN_POINT('',(219.182069373787,67.2397376070391,358.164796223596));
#24971=CARTESIAN_POINT('',(190.689220941112,65.2397376070391,351.630177842849));
#24972=CARTESIAN_POINT('',(219.182069373787,65.2397376070391,358.164796223596));
#24973=CARTESIAN_POINT('',(201.245093613437,37.0155488911437,354.051087066874));
#24974=CARTESIAN_POINT('',(201.245093613437,37.0155488911437,354.051087066874));
#24975=CARTESIAN_POINT('Origin',(209.435119279911,40.2397376070391,355.929407249055));
#24976=CARTESIAN_POINT('Origin',(219.852686066149,31.2397376070391,355.240711195433));
#24977=CARTESIAN_POINT('',(191.359837633474,65.2397376070391,348.706092814686));
#24978=CARTESIAN_POINT('',(201.915710305799,37.0155488911437,351.127002038711));
#24979=CARTESIAN_POINT('',(206.100637103286,25.8259327067678,352.086783214593));
#24980=CARTESIAN_POINT('',(219.780926546604,65.2397376070391,355.224253694649));
#24981=CARTESIAN_POINT('',(219.852686066149,65.2397376070391,355.240711195433));
#24982=CARTESIAN_POINT('',(218.872053582717,39.9086604301851,355.015810583403));
#24983=CARTESIAN_POINT('',(218.562762650207,31.2884540946096,354.944877057141));
#24984=CARTESIAN_POINT('Origin',(210.105735972273,40.2397376070391,353.005322220892));
#24985=CARTESIAN_POINT('Origin',(225.217619605046,67.2397376070391,331.848030970131));
#24986=CARTESIAN_POINT('',(224.770541810138,67.2397376070391,333.797420988906));
#24987=CARTESIAN_POINT('',(220.299763861057,67.2397376070391,353.291321176658));
#24988=CARTESIAN_POINT('',(225.217619605046,67.2397376070391,331.848030970131));
#24989=CARTESIAN_POINT('',(191.05891357943,67.2397376070391,346.585154253036));
#24990=CARTESIAN_POINT('',(191.05891357943,67.2397376070391,346.585154253036));
#24991=CARTESIAN_POINT('',(195.529691528511,67.2397376070391,327.091254065285));
#24992=CARTESIAN_POINT('',(195.97676932342,67.2397376070391,325.14186404651));
#24993=CARTESIAN_POINT('',(224.770541810138,67.2397376070391,333.797420988906));
#24994=CARTESIAN_POINT('Origin',(222.535152835598,31.2397376070391,343.544371082782));
#24995=CARTESIAN_POINT('',(225.794925728488,67.2397376070391,329.330807328892));
#24996=CARTESIAN_POINT('',(225.888236297409,67.2397376070391,328.923945941969));
#24997=CARTESIAN_POINT('Origin',(224.770541810138,65.2397376070391,333.797420988906));
#24998=CARTESIAN_POINT('',(219.275379942707,67.2397376070391,357.757934836672));
#24999=CARTESIAN_POINT('Origin',(220.299763861057,65.2397376070391,353.291321176658));
#25000=CARTESIAN_POINT('',(222.535152835598,67.2397376070391,343.544371082782));
#25001=CARTESIAN_POINT('Origin',(193.294302553971,31.2397376070391,336.83820415916));
#25002=CARTESIAN_POINT('',(196.554075446862,67.2397376070391,322.62464040527));
#25003=CARTESIAN_POINT('Origin',(195.529691528511,65.2397376070391,327.091254065285));
#25004=CARTESIAN_POINT('',(196.647386015782,67.2397376070391,322.217779018347));
#25005=CARTESIAN_POINT('',(190.03452966108,67.2397376070391,351.05176791305));
#25006=CARTESIAN_POINT('',(193.294302553971,67.2397376070391,336.83820415916));
#25007=CARTESIAN_POINT('Origin',(191.05891357943,65.2397376070391,346.585154253036));
#25008=CARTESIAN_POINT('Origin',(207.951260537059,37.0155488911437,324.810236785247));
#25009=CARTESIAN_POINT('Origin',(191.806915428346,65.2397376070675,346.756702796012));
#25010=CARTESIAN_POINT('Origin',(191.806915428382,65.2397376070398,346.756702795912));
#25011=CARTESIAN_POINT('',(207.951260537059,37.0155488911437,324.810236785247));
#25012=CARTESIAN_POINT('Origin',(225.888236297409,67.2397376070391,328.923945941969));
#25013=CARTESIAN_POINT('Origin',(220.228004341512,65.2397376070391,353.274863675874));
#25014=CARTESIAN_POINT('',(224.907603813977,39.9086604301851,328.699045329938));
#25015=CARTESIAN_POINT('Origin',(220.228004341512,65.2397376070392,353.274863675875));
#25016=CARTESIAN_POINT('Origin',(216.141286203533,40.2397376070391,326.688556967428));
#25017=CARTESIAN_POINT('Origin',(216.141286203533,40.2397376070391,326.688556967428));
#25018=CARTESIAN_POINT('',(207.951260537059,37.0155488911437,324.810236785247));
#25019=CARTESIAN_POINT('',(224.907603813977,39.9086604301851,328.699045329938));
#25020=CARTESIAN_POINT('Origin',(225.888236297409,67.2397376070391,328.923945941969));
#25021=CARTESIAN_POINT('Origin',(224.698782290593,65.2397376070391,333.780963488123));
#25022=CARTESIAN_POINT('Origin',(224.698782290594,65.2397376070431,333.780963488119));
#25023=CARTESIAN_POINT('Origin',(207.951260537059,37.0155488911437,324.810236785247));
#25024=CARTESIAN_POINT('Origin',(196.27769337772,65.2397376073992,327.262802606412));
#25025=CARTESIAN_POINT('Origin',(196.277693377464,65.2397376070354,327.262802608164));
#25026=CARTESIAN_POINT('Origin',(193.294302553971,85.7397376070391,336.83820415916));
#25027=CARTESIAN_POINT('Origin',(198.167777600909,100.739737607039,337.955898646431));
#25028=CARTESIAN_POINT('Origin',(204.098450146653,87.9334876077219,334.46390266032));
#25029=CARTESIAN_POINT('',(204.098450146653,87.9334876077219,334.46390266032));
#25030=CARTESIAN_POINT('',(204.098450146653,87.3709876090875,334.46390266032));
#25031=CARTESIAN_POINT('Ctrl Pts',(204.03795315819,101.777237608405,334.727687233877));
#25032=CARTESIAN_POINT('Ctrl Pts',(205.838086322694,101.714737608405,335.140534102886));
#25033=CARTESIAN_POINT('Ctrl Pts',(206.819045869686,101.652237608405,336.705347291213));
#25034=CARTESIAN_POINT('Ctrl Pts',(207.800005416678,101.589737608405,338.27016047954));
#25035=CARTESIAN_POINT('Ctrl Pts',(207.38715854767,101.527237608405,340.070293644044));
#25036=CARTESIAN_POINT('Ctrl Pts',(206.974311678662,101.464737608405,341.870426808548));
#25037=CARTESIAN_POINT('Ctrl Pts',(205.409498490334,101.402237608405,342.851386355541));
#25038=CARTESIAN_POINT('Ctrl Pts',(203.844685302007,101.339737608405,343.832345902533));
#25039=CARTESIAN_POINT('Ctrl Pts',(202.044552137503,101.277237608405,343.419499033524));
#25040=CARTESIAN_POINT('Ctrl Pts',(200.244418972999,101.214737608405,343.006652164516));
#25041=CARTESIAN_POINT('Ctrl Pts',(199.263459426007,101.152237608405,341.441838976189));
#25042=CARTESIAN_POINT('Ctrl Pts',(198.282499879015,101.089737608405,339.877025787862));
#25043=CARTESIAN_POINT('Ctrl Pts',(198.695346748023,101.027237608405,338.076892623358));
#25044=CARTESIAN_POINT('Ctrl Pts',(199.108193617031,100.964737608405,336.276759458854));
#25045=CARTESIAN_POINT('Ctrl Pts',(200.673006805358,100.902237608405,335.295799911861));
#25046=CARTESIAN_POINT('Ctrl Pts',(202.237819993686,100.839737608405,334.314840364869));
#25047=CARTESIAN_POINT('Ctrl Pts',(204.03795315819,100.777237608405,334.727687233877));
#25048=CARTESIAN_POINT('Ctrl Pts',(205.838086322694,100.714737608405,335.140534102886));
#25049=CARTESIAN_POINT('Ctrl Pts',(206.819045869686,100.652237608405,336.705347291213));
#25050=CARTESIAN_POINT('Ctrl Pts',(207.800005416678,100.589737608405,338.27016047954));
#25051=CARTESIAN_POINT('Ctrl Pts',(207.38715854767,100.527237608405,340.070293644044));
#25052=CARTESIAN_POINT('Ctrl Pts',(206.974311678662,100.464737608405,341.870426808548));
#25053=CARTESIAN_POINT('Ctrl Pts',(205.409498490334,100.402237608405,342.851386355541));
#25054=CARTESIAN_POINT('Ctrl Pts',(203.844685302007,100.339737608405,343.832345902533));
#25055=CARTESIAN_POINT('Ctrl Pts',(202.044552137503,100.277237608405,343.419499033524));
#25056=CARTESIAN_POINT('Ctrl Pts',(200.244418972999,100.214737608405,343.006652164516));
#25057=CARTESIAN_POINT('Ctrl Pts',(199.263459426007,100.152237608405,341.441838976189));
#25058=CARTESIAN_POINT('Ctrl Pts',(198.282499879015,100.089737608405,339.877025787862));
#25059=CARTESIAN_POINT('Ctrl Pts',(198.695346748023,100.027237608405,338.076892623358));
#25060=CARTESIAN_POINT('Ctrl Pts',(199.108193617031,99.9647376084047,336.276759458854));
#25061=CARTESIAN_POINT('Ctrl Pts',(200.673006805358,99.9022376084047,335.295799911861));
#25062=CARTESIAN_POINT('Ctrl Pts',(202.237819993686,99.8397376084047,334.314840364869));
#25063=CARTESIAN_POINT('Ctrl Pts',(204.03795315819,99.7772376084047,334.727687233877));
#25064=CARTESIAN_POINT('Ctrl Pts',(205.838086322694,99.7147376084047,335.140534102886));
#25065=CARTESIAN_POINT('Ctrl Pts',(206.819045869686,99.6522376084047,336.705347291213));
#25066=CARTESIAN_POINT('Ctrl Pts',(207.800005416678,99.5897376084047,338.27016047954));
#25067=CARTESIAN_POINT('Ctrl Pts',(207.38715854767,99.5272376084047,340.070293644044));
#25068=CARTESIAN_POINT('Ctrl Pts',(206.974311678662,99.4647376084047,341.870426808548));
#25069=CARTESIAN_POINT('Ctrl Pts',(205.409498490334,99.4022376084047,342.851386355541));
#25070=CARTESIAN_POINT('Ctrl Pts',(203.844685302007,99.3397376084047,343.832345902533));
#25071=CARTESIAN_POINT('Ctrl Pts',(202.044552137503,99.2772376084047,343.419499033524));
#25072=CARTESIAN_POINT('Ctrl Pts',(200.244418972999,99.2147376084047,343.006652164516));
#25073=CARTESIAN_POINT('Ctrl Pts',(199.263459426007,99.1522376084047,341.441838976189));
#25074=CARTESIAN_POINT('Ctrl Pts',(198.282499879015,99.0897376084047,339.877025787862));
#25075=CARTESIAN_POINT('Ctrl Pts',(198.695346748023,99.0272376084047,338.076892623358));
#25076=CARTESIAN_POINT('Ctrl Pts',(199.108193617031,98.9647376084047,336.276759458854));
#25077=CARTESIAN_POINT('Ctrl Pts',(200.673006805358,98.9022376084047,335.295799911861));
#25078=CARTESIAN_POINT('Ctrl Pts',(202.237819993686,98.8397376084047,334.314840364869));
#25079=CARTESIAN_POINT('Ctrl Pts',(204.03795315819,98.7772376084047,334.727687233877));
#25080=CARTESIAN_POINT('Ctrl Pts',(205.838086322694,98.7147376084047,335.140534102886));
#25081=CARTESIAN_POINT('Ctrl Pts',(206.819045869686,98.6522376084047,336.705347291213));
#25082=CARTESIAN_POINT('Ctrl Pts',(207.800005416678,98.5897376084047,338.27016047954));
#25083=CARTESIAN_POINT('Ctrl Pts',(207.38715854767,98.5272376084047,340.070293644044));
#25084=CARTESIAN_POINT('Ctrl Pts',(206.974311678662,98.4647376084047,341.870426808548));
#25085=CARTESIAN_POINT('Ctrl Pts',(205.409498490334,98.4022376084047,342.851386355541));
#25086=CARTESIAN_POINT('Ctrl Pts',(203.844685302007,98.3397376084047,343.832345902533));
#25087=CARTESIAN_POINT('Ctrl Pts',(202.044552137503,98.2772376084047,343.419499033524));
#25088=CARTESIAN_POINT('Ctrl Pts',(200.244418972999,98.2147376084047,343.006652164516));
#25089=CARTESIAN_POINT('Ctrl Pts',(199.263459426007,98.1522376084047,341.441838976189));
#25090=CARTESIAN_POINT('Ctrl Pts',(198.282499879015,98.0897376084047,339.877025787862));
#25091=CARTESIAN_POINT('Ctrl Pts',(198.695346748023,98.0272376084047,338.076892623358));
#25092=CARTESIAN_POINT('Ctrl Pts',(199.108193617031,97.9647376084047,336.276759458854));
#25093=CARTESIAN_POINT('Ctrl Pts',(200.673006805358,97.9022376084047,335.295799911861));
#25094=CARTESIAN_POINT('Ctrl Pts',(202.237819993686,97.8397376084047,334.314840364869));
#25095=CARTESIAN_POINT('Ctrl Pts',(204.03795315819,97.7772376084047,334.727687233877));
#25096=CARTESIAN_POINT('Ctrl Pts',(205.838086322694,97.7147376084047,335.140534102886));
#25097=CARTESIAN_POINT('Ctrl Pts',(206.819045869686,97.6522376084047,336.705347291213));
#25098=CARTESIAN_POINT('Ctrl Pts',(207.800005416678,97.5897376084047,338.27016047954));
#25099=CARTESIAN_POINT('Ctrl Pts',(207.38715854767,97.5272376084047,340.070293644044));
#25100=CARTESIAN_POINT('Ctrl Pts',(206.974311678662,97.4647376084047,341.870426808548));
#25101=CARTESIAN_POINT('Ctrl Pts',(205.409498490334,97.4022376084047,342.851386355541));
#25102=CARTESIAN_POINT('Ctrl Pts',(203.844685302007,97.3397376084047,343.832345902533));
#25103=CARTESIAN_POINT('Ctrl Pts',(202.044552137503,97.2772376084047,343.419499033524));
#25104=CARTESIAN_POINT('Ctrl Pts',(200.244418972999,97.2147376084047,343.006652164516));
#25105=CARTESIAN_POINT('Ctrl Pts',(199.263459426007,97.1522376084047,341.441838976189));
#25106=CARTESIAN_POINT('Ctrl Pts',(198.282499879015,97.0897376084047,339.877025787862));
#25107=CARTESIAN_POINT('Ctrl Pts',(198.695346748023,97.0272376084047,338.076892623358));
#25108=CARTESIAN_POINT('Ctrl Pts',(199.108193617031,96.9647376084047,336.276759458854));
#25109=CARTESIAN_POINT('Ctrl Pts',(200.673006805358,96.9022376084047,335.295799911861));
#25110=CARTESIAN_POINT('Ctrl Pts',(202.237819993686,96.8397376084047,334.314840364869));
#25111=CARTESIAN_POINT('Ctrl Pts',(204.03795315819,96.7772376084047,334.727687233877));
#25112=CARTESIAN_POINT('Ctrl Pts',(205.838086322694,96.7147376084047,335.140534102886));
#25113=CARTESIAN_POINT('Ctrl Pts',(206.819045869686,96.6522376084047,336.705347291213));
#25114=CARTESIAN_POINT('Ctrl Pts',(207.800005416678,96.5897376084047,338.27016047954));
#25115=CARTESIAN_POINT('Ctrl Pts',(207.38715854767,96.5272376084047,340.070293644044));
#25116=CARTESIAN_POINT('Ctrl Pts',(206.974311678662,96.4647376084047,341.870426808548));
#25117=CARTESIAN_POINT('Ctrl Pts',(205.409498490334,96.4022376084047,342.851386355541));
#25118=CARTESIAN_POINT('Ctrl Pts',(203.844685302007,96.3397376084047,343.832345902533));
#25119=CARTESIAN_POINT('Ctrl Pts',(202.044552137503,96.2772376084047,343.419499033524));
#25120=CARTESIAN_POINT('Ctrl Pts',(200.244418972999,96.2147376084047,343.006652164516));
#25121=CARTESIAN_POINT('Ctrl Pts',(199.263459426007,96.1522376084047,341.441838976189));
#25122=CARTESIAN_POINT('Ctrl Pts',(198.282499879015,96.0897376084047,339.877025787862));
#25123=CARTESIAN_POINT('Ctrl Pts',(198.695346748023,96.0272376084047,338.076892623358));
#25124=CARTESIAN_POINT('Ctrl Pts',(199.108193617031,95.9647376084047,336.276759458854));
#25125=CARTESIAN_POINT('Ctrl Pts',(200.673006805358,95.9022376084047,335.295799911861));
#25126=CARTESIAN_POINT('Ctrl Pts',(202.237819993686,95.8397376084047,334.314840364869));
#25127=CARTESIAN_POINT('Ctrl Pts',(204.03795315819,95.7772376084047,334.727687233877));
#25128=CARTESIAN_POINT('Ctrl Pts',(205.838086322694,95.7147376084047,335.140534102886));
#25129=CARTESIAN_POINT('Ctrl Pts',(206.819045869686,95.6522376084047,336.705347291213));
#25130=CARTESIAN_POINT('Ctrl Pts',(207.800005416678,95.5897376084047,338.27016047954));
#25131=CARTESIAN_POINT('Ctrl Pts',(207.38715854767,95.5272376084047,340.070293644044));
#25132=CARTESIAN_POINT('Ctrl Pts',(206.974311678662,95.4647376084047,341.870426808548));
#25133=CARTESIAN_POINT('Ctrl Pts',(205.409498490334,95.4022376084047,342.851386355541));
#25134=CARTESIAN_POINT('Ctrl Pts',(203.844685302007,95.3397376084047,343.832345902533));
#25135=CARTESIAN_POINT('Ctrl Pts',(202.044552137503,95.2772376084047,343.419499033524));
#25136=CARTESIAN_POINT('Ctrl Pts',(200.244418972999,95.2147376084047,343.006652164516));
#25137=CARTESIAN_POINT('Ctrl Pts',(199.263459426007,95.1522376084047,341.441838976189));
#25138=CARTESIAN_POINT('Ctrl Pts',(198.282499879015,95.0897376084047,339.877025787862));
#25139=CARTESIAN_POINT('Ctrl Pts',(198.695346748023,95.0272376084047,338.076892623358));
#25140=CARTESIAN_POINT('Ctrl Pts',(199.108193617031,94.9647376084047,336.276759458854));
#25141=CARTESIAN_POINT('Ctrl Pts',(200.673006805358,94.9022376084047,335.295799911861));
#25142=CARTESIAN_POINT('Ctrl Pts',(202.237819993686,94.8397376084047,334.314840364869));
#25143=CARTESIAN_POINT('Ctrl Pts',(204.03795315819,94.7772376084047,334.727687233877));
#25144=CARTESIAN_POINT('Ctrl Pts',(205.838086322694,94.7147376084047,335.140534102886));
#25145=CARTESIAN_POINT('Ctrl Pts',(206.819045869686,94.6522376084047,336.705347291213));
#25146=CARTESIAN_POINT('Ctrl Pts',(207.800005416678,94.5897376084047,338.27016047954));
#25147=CARTESIAN_POINT('Ctrl Pts',(207.38715854767,94.5272376084047,340.070293644044));
#25148=CARTESIAN_POINT('Ctrl Pts',(206.974311678662,94.4647376084047,341.870426808548));
#25149=CARTESIAN_POINT('Ctrl Pts',(205.409498490334,94.4022376084047,342.851386355541));
#25150=CARTESIAN_POINT('Ctrl Pts',(203.844685302007,94.3397376084047,343.832345902533));
#25151=CARTESIAN_POINT('Ctrl Pts',(202.044552137503,94.2772376084047,343.419499033524));
#25152=CARTESIAN_POINT('Ctrl Pts',(200.244418972999,94.2147376084047,343.006652164516));
#25153=CARTESIAN_POINT('Ctrl Pts',(199.263459426007,94.1522376084047,341.441838976189));
#25154=CARTESIAN_POINT('Ctrl Pts',(198.282499879015,94.0897376084047,339.877025787862));
#25155=CARTESIAN_POINT('Ctrl Pts',(198.695346748023,94.0272376084047,338.076892623358));
#25156=CARTESIAN_POINT('Ctrl Pts',(199.108193617031,93.9647376084047,336.276759458854));
#25157=CARTESIAN_POINT('Ctrl Pts',(200.673006805358,93.9022376084047,335.295799911861));
#25158=CARTESIAN_POINT('Ctrl Pts',(202.237819993686,93.8397376084047,334.314840364869));
#25159=CARTESIAN_POINT('Ctrl Pts',(204.03795315819,93.7772376084047,334.727687233877));
#25160=CARTESIAN_POINT('Ctrl Pts',(205.838086322694,93.7147376084047,335.140534102886));
#25161=CARTESIAN_POINT('Ctrl Pts',(206.819045869686,93.6522376084047,336.705347291213));
#25162=CARTESIAN_POINT('Ctrl Pts',(207.800005416678,93.5897376084047,338.27016047954));
#25163=CARTESIAN_POINT('Ctrl Pts',(207.38715854767,93.5272376084047,340.070293644044));
#25164=CARTESIAN_POINT('Ctrl Pts',(206.974311678662,93.4647376084047,341.870426808548));
#25165=CARTESIAN_POINT('Ctrl Pts',(205.409498490334,93.4022376084047,342.851386355541));
#25166=CARTESIAN_POINT('Ctrl Pts',(203.844685302007,93.3397376084047,343.832345902533));
#25167=CARTESIAN_POINT('Ctrl Pts',(202.044552137503,93.2772376084047,343.419499033524));
#25168=CARTESIAN_POINT('Ctrl Pts',(200.244418972999,93.2147376084047,343.006652164516));
#25169=CARTESIAN_POINT('Ctrl Pts',(199.263459426007,93.1522376084047,341.441838976189));
#25170=CARTESIAN_POINT('Ctrl Pts',(198.282499879015,93.0897376084047,339.877025787862));
#25171=CARTESIAN_POINT('Ctrl Pts',(198.695346748023,93.0272376084047,338.076892623358));
#25172=CARTESIAN_POINT('Ctrl Pts',(199.108193617031,92.9647376084047,336.276759458854));
#25173=CARTESIAN_POINT('Ctrl Pts',(200.673006805358,92.9022376084047,335.295799911861));
#25174=CARTESIAN_POINT('Ctrl Pts',(202.237819993686,92.8397376084047,334.314840364869));
#25175=CARTESIAN_POINT('Ctrl Pts',(204.03795315819,92.7772376084047,334.727687233877));
#25176=CARTESIAN_POINT('Ctrl Pts',(205.838086322694,92.7147376084047,335.140534102886));
#25177=CARTESIAN_POINT('Ctrl Pts',(206.819045869686,92.6522376084047,336.705347291213));
#25178=CARTESIAN_POINT('Ctrl Pts',(207.800005416678,92.5897376084047,338.27016047954));
#25179=CARTESIAN_POINT('Ctrl Pts',(207.38715854767,92.5272376084047,340.070293644044));
#25180=CARTESIAN_POINT('Ctrl Pts',(206.974311678662,92.4647376084047,341.870426808548));
#25181=CARTESIAN_POINT('Ctrl Pts',(205.409498490334,92.4022376084047,342.851386355541));
#25182=CARTESIAN_POINT('Ctrl Pts',(203.844685302007,92.3397376084047,343.832345902533));
#25183=CARTESIAN_POINT('Ctrl Pts',(202.044552137503,92.2772376084047,343.419499033524));
#25184=CARTESIAN_POINT('Ctrl Pts',(200.244418972999,92.2147376084047,343.006652164516));
#25185=CARTESIAN_POINT('Ctrl Pts',(199.263459426007,92.1522376084047,341.441838976189));
#25186=CARTESIAN_POINT('Ctrl Pts',(198.282499879015,92.0897376084047,339.877025787862));
#25187=CARTESIAN_POINT('Ctrl Pts',(198.695346748023,92.0272376084047,338.076892623358));
#25188=CARTESIAN_POINT('Ctrl Pts',(199.108193617031,91.9647376084047,336.276759458854));
#25189=CARTESIAN_POINT('Ctrl Pts',(200.673006805358,91.9022376084047,335.295799911861));
#25190=CARTESIAN_POINT('Ctrl Pts',(202.237819993686,91.8397376084047,334.314840364869));
#25191=CARTESIAN_POINT('Ctrl Pts',(204.03795315819,91.7772376084047,334.727687233877));
#25192=CARTESIAN_POINT('Ctrl Pts',(205.838086322694,91.7147376084047,335.140534102886));
#25193=CARTESIAN_POINT('Ctrl Pts',(206.819045869686,91.6522376084047,336.705347291213));
#25194=CARTESIAN_POINT('Ctrl Pts',(207.800005416678,91.5897376084047,338.27016047954));
#25195=CARTESIAN_POINT('Ctrl Pts',(207.38715854767,91.5272376084047,340.070293644044));
#25196=CARTESIAN_POINT('Ctrl Pts',(206.974311678662,91.4647376084047,341.870426808548));
#25197=CARTESIAN_POINT('Ctrl Pts',(205.409498490334,91.4022376084047,342.851386355541));
#25198=CARTESIAN_POINT('Ctrl Pts',(203.844685302007,91.3397376084047,343.832345902533));
#25199=CARTESIAN_POINT('Ctrl Pts',(202.044552137503,91.2772376084047,343.419499033524));
#25200=CARTESIAN_POINT('Ctrl Pts',(200.244418972999,91.2147376084047,343.006652164516));
#25201=CARTESIAN_POINT('Ctrl Pts',(199.263459426007,91.1522376084047,341.441838976189));
#25202=CARTESIAN_POINT('Ctrl Pts',(198.282499879015,91.0897376084047,339.877025787862));
#25203=CARTESIAN_POINT('Ctrl Pts',(198.695346748023,91.0272376084047,338.076892623358));
#25204=CARTESIAN_POINT('Ctrl Pts',(199.108193617031,90.9647376084047,336.276759458854));
#25205=CARTESIAN_POINT('Ctrl Pts',(200.673006805358,90.9022376084047,335.295799911861));
#25206=CARTESIAN_POINT('Ctrl Pts',(202.237819993686,90.8397376084047,334.314840364869));
#25207=CARTESIAN_POINT('Ctrl Pts',(204.03795315819,90.7772376084047,334.727687233877));
#25208=CARTESIAN_POINT('Ctrl Pts',(205.838086322694,90.7147376084047,335.140534102886));
#25209=CARTESIAN_POINT('Ctrl Pts',(206.819045869686,90.6522376084047,336.705347291213));
#25210=CARTESIAN_POINT('Ctrl Pts',(207.800005416678,90.5897376084047,338.27016047954));
#25211=CARTESIAN_POINT('Ctrl Pts',(207.38715854767,90.5272376084047,340.070293644044));
#25212=CARTESIAN_POINT('Ctrl Pts',(206.974311678662,90.4647376084047,341.870426808548));
#25213=CARTESIAN_POINT('Ctrl Pts',(205.409498490334,90.4022376084047,342.851386355541));
#25214=CARTESIAN_POINT('Ctrl Pts',(203.844685302007,90.3397376084047,343.832345902533));
#25215=CARTESIAN_POINT('Ctrl Pts',(202.044552137503,90.2772376084047,343.419499033524));
#25216=CARTESIAN_POINT('Ctrl Pts',(200.244418972999,90.2147376084047,343.006652164516));
#25217=CARTESIAN_POINT('Ctrl Pts',(199.263459426007,90.1522376084047,341.441838976189));
#25218=CARTESIAN_POINT('Ctrl Pts',(198.282499879015,90.0897376084047,339.877025787862));
#25219=CARTESIAN_POINT('Ctrl Pts',(198.695346748023,90.0272376084047,338.076892623358));
#25220=CARTESIAN_POINT('Ctrl Pts',(199.108193617031,89.9647376084047,336.276759458854));
#25221=CARTESIAN_POINT('Ctrl Pts',(200.673006805358,89.9022376084047,335.295799911861));
#25222=CARTESIAN_POINT('Ctrl Pts',(202.237819993686,89.8397376084047,334.314840364869));
#25223=CARTESIAN_POINT('Ctrl Pts',(204.03795315819,89.7772376084047,334.727687233877));
#25224=CARTESIAN_POINT('Ctrl Pts',(205.838086322694,89.7147376084047,335.140534102886));
#25225=CARTESIAN_POINT('Ctrl Pts',(206.819045869686,89.6522376084047,336.705347291213));
#25226=CARTESIAN_POINT('Ctrl Pts',(207.800005416678,89.5897376084047,338.27016047954));
#25227=CARTESIAN_POINT('Ctrl Pts',(207.38715854767,89.5272376084047,340.070293644044));
#25228=CARTESIAN_POINT('Ctrl Pts',(206.974311678662,89.4647376084047,341.870426808548));
#25229=CARTESIAN_POINT('Ctrl Pts',(205.409498490334,89.4022376084047,342.851386355541));
#25230=CARTESIAN_POINT('Ctrl Pts',(203.844685302007,89.3397376084047,343.832345902533));
#25231=CARTESIAN_POINT('Ctrl Pts',(202.044552137503,89.2772376084047,343.419499033524));
#25232=CARTESIAN_POINT('Ctrl Pts',(200.244418972999,89.2147376084047,343.006652164516));
#25233=CARTESIAN_POINT('Ctrl Pts',(199.263459426007,89.1522376084047,341.441838976189));
#25234=CARTESIAN_POINT('Ctrl Pts',(198.282499879015,89.0897376084047,339.877025787862));
#25235=CARTESIAN_POINT('Ctrl Pts',(198.695346748023,89.0272376084047,338.076892623358));
#25236=CARTESIAN_POINT('Ctrl Pts',(199.108193617031,88.9647376084047,336.276759458854));
#25237=CARTESIAN_POINT('Ctrl Pts',(200.673006805358,88.9022376084047,335.295799911861));
#25238=CARTESIAN_POINT('Ctrl Pts',(202.237819993686,88.8397376084047,334.314840364869));
#25239=CARTESIAN_POINT('Ctrl Pts',(204.03795315819,88.7772376084047,334.727687233877));
#25240=CARTESIAN_POINT('Ctrl Pts',(205.838086322694,88.7147376084047,335.140534102886));
#25241=CARTESIAN_POINT('Ctrl Pts',(206.819045869686,88.6522376084047,336.705347291213));
#25242=CARTESIAN_POINT('Ctrl Pts',(207.800005416678,88.5897376084047,338.27016047954));
#25243=CARTESIAN_POINT('Ctrl Pts',(207.38715854767,88.5272376084047,340.070293644044));
#25244=CARTESIAN_POINT('Ctrl Pts',(206.974311678662,88.4647376084047,341.870426808548));
#25245=CARTESIAN_POINT('Ctrl Pts',(205.409498490334,88.4022376084047,342.851386355541));
#25246=CARTESIAN_POINT('Ctrl Pts',(203.844685302007,88.3397376084047,343.832345902533));
#25247=CARTESIAN_POINT('Ctrl Pts',(202.044552137503,88.2772376084047,343.419499033524));
#25248=CARTESIAN_POINT('Ctrl Pts',(200.244418972999,88.2147376084047,343.006652164516));
#25249=CARTESIAN_POINT('Ctrl Pts',(199.263459426007,88.1522376084047,341.441838976189));
#25250=CARTESIAN_POINT('Ctrl Pts',(198.282499879015,88.0897376084047,339.877025787862));
#25251=CARTESIAN_POINT('Ctrl Pts',(198.695346748023,88.0272376084047,338.076892623358));
#25252=CARTESIAN_POINT('Ctrl Pts',(199.108193617031,87.9647376084047,336.276759458854));
#25253=CARTESIAN_POINT('Ctrl Pts',(200.673006805358,87.9022376084047,335.295799911861));
#25254=CARTESIAN_POINT('Ctrl Pts',(202.237819993686,87.8397376084047,334.314840364869));
#25255=CARTESIAN_POINT('Ctrl Pts',(204.03795315819,87.7772376084047,334.727687233877));
#25256=CARTESIAN_POINT('Ctrl Pts',(204.158947322422,102.089738090806,334.200117270057));
#25257=CARTESIAN_POINT('Ctrl Pts',(206.177607121041,102.027238090806,334.663081562858));
#25258=CARTESIAN_POINT('Ctrl Pts',(207.277649962667,101.964738090806,336.417854786258));
#25259=CARTESIAN_POINT('Ctrl Pts',(208.377692804292,101.902238090806,338.172628009657));
#25260=CARTESIAN_POINT('Ctrl Pts',(207.914728511491,101.839738090806,340.191287808277));
#25261=CARTESIAN_POINT('Ctrl Pts',(207.451764218689,101.777238090806,342.209947606896));
#25262=CARTESIAN_POINT('Ctrl Pts',(205.69699099529,101.714738090806,343.309990448521));
#25263=CARTESIAN_POINT('Ctrl Pts',(203.94221777189,101.652238090806,344.410033290147));
#25264=CARTESIAN_POINT('Ctrl Pts',(201.923557973271,101.589738090806,343.947068997345));
#25265=CARTESIAN_POINT('Ctrl Pts',(199.904898174651,101.527238090806,343.484104704544));
#25266=CARTESIAN_POINT('Ctrl Pts',(198.804855333026,101.464738090806,341.729331481144));
#25267=CARTESIAN_POINT('Ctrl Pts',(197.704812491401,101.402238090806,339.974558257745));
#25268=CARTESIAN_POINT('Ctrl Pts',(198.167776784202,101.339738090806,337.955898459125));
#25269=CARTESIAN_POINT('Ctrl Pts',(198.630741077004,101.277238090806,335.937238660506));
#25270=CARTESIAN_POINT('Ctrl Pts',(200.385514300403,101.214738090806,334.837195818881));
#25271=CARTESIAN_POINT('Ctrl Pts',(202.140287523803,101.152238090806,333.737152977255));
#25272=CARTESIAN_POINT('Ctrl Pts',(204.158947322422,101.089738090806,334.200117270057));
#25273=CARTESIAN_POINT('Ctrl Pts',(206.177607121041,101.027238090806,334.663081562858));
#25274=CARTESIAN_POINT('Ctrl Pts',(207.277649962667,100.964738090806,336.417854786258));
#25275=CARTESIAN_POINT('Ctrl Pts',(208.377692804292,100.902238090806,338.172628009657));
#25276=CARTESIAN_POINT('Ctrl Pts',(207.914728511491,100.839738090806,340.191287808277));
#25277=CARTESIAN_POINT('Ctrl Pts',(207.451764218689,100.777238090806,342.209947606896));
#25278=CARTESIAN_POINT('Ctrl Pts',(205.69699099529,100.714738090806,343.309990448521));
#25279=CARTESIAN_POINT('Ctrl Pts',(203.94221777189,100.652238090806,344.410033290147));
#25280=CARTESIAN_POINT('Ctrl Pts',(201.923557973271,100.589738090806,343.947068997345));
#25281=CARTESIAN_POINT('Ctrl Pts',(199.904898174651,100.527238090806,343.484104704544));
#25282=CARTESIAN_POINT('Ctrl Pts',(198.804855333026,100.464738090806,341.729331481144));
#25283=CARTESIAN_POINT('Ctrl Pts',(197.704812491401,100.402238090806,339.974558257745));
#25284=CARTESIAN_POINT('Ctrl Pts',(198.167776784202,100.339738090806,337.955898459125));
#25285=CARTESIAN_POINT('Ctrl Pts',(198.630741077004,100.277238090806,335.937238660506));
#25286=CARTESIAN_POINT('Ctrl Pts',(200.385514300403,100.214738090806,334.837195818881));
#25287=CARTESIAN_POINT('Ctrl Pts',(202.140287523803,100.152238090806,333.737152977255));
#25288=CARTESIAN_POINT('Ctrl Pts',(204.158947322422,100.089738090806,334.200117270057));
#25289=CARTESIAN_POINT('Ctrl Pts',(206.177607121041,100.027238090806,334.663081562858));
#25290=CARTESIAN_POINT('Ctrl Pts',(207.277649962667,99.9647380908064,336.417854786258));
#25291=CARTESIAN_POINT('Ctrl Pts',(208.377692804292,99.9022380908064,338.172628009657));
#25292=CARTESIAN_POINT('Ctrl Pts',(207.914728511491,99.8397380908065,340.191287808277));
#25293=CARTESIAN_POINT('Ctrl Pts',(207.451764218689,99.7772380908064,342.209947606896));
#25294=CARTESIAN_POINT('Ctrl Pts',(205.69699099529,99.7147380908064,343.309990448521));
#25295=CARTESIAN_POINT('Ctrl Pts',(203.94221777189,99.6522380908065,344.410033290147));
#25296=CARTESIAN_POINT('Ctrl Pts',(201.923557973271,99.5897380908065,343.947068997345));
#25297=CARTESIAN_POINT('Ctrl Pts',(199.904898174651,99.5272380908065,343.484104704544));
#25298=CARTESIAN_POINT('Ctrl Pts',(198.804855333026,99.4647380908065,341.729331481144));
#25299=CARTESIAN_POINT('Ctrl Pts',(197.704812491401,99.4022380908064,339.974558257745));
#25300=CARTESIAN_POINT('Ctrl Pts',(198.167776784202,99.3397380908064,337.955898459125));
#25301=CARTESIAN_POINT('Ctrl Pts',(198.630741077004,99.2772380908065,335.937238660506));
#25302=CARTESIAN_POINT('Ctrl Pts',(200.385514300403,99.2147380908065,334.837195818881));
#25303=CARTESIAN_POINT('Ctrl Pts',(202.140287523803,99.1522380908065,333.737152977255));
#25304=CARTESIAN_POINT('Ctrl Pts',(204.158947322422,99.0897380908064,334.200117270057));
#25305=CARTESIAN_POINT('Ctrl Pts',(206.177607121041,99.0272380908065,334.663081562858));
#25306=CARTESIAN_POINT('Ctrl Pts',(207.277649962667,98.9647380908064,336.417854786258));
#25307=CARTESIAN_POINT('Ctrl Pts',(208.377692804292,98.9022380908064,338.172628009657));
#25308=CARTESIAN_POINT('Ctrl Pts',(207.914728511491,98.8397380908065,340.191287808277));
#25309=CARTESIAN_POINT('Ctrl Pts',(207.451764218689,98.7772380908064,342.209947606896));
#25310=CARTESIAN_POINT('Ctrl Pts',(205.69699099529,98.7147380908064,343.309990448521));
#25311=CARTESIAN_POINT('Ctrl Pts',(203.94221777189,98.6522380908065,344.410033290147));
#25312=CARTESIAN_POINT('Ctrl Pts',(201.923557973271,98.5897380908064,343.947068997345));
#25313=CARTESIAN_POINT('Ctrl Pts',(199.904898174651,98.5272380908065,343.484104704544));
#25314=CARTESIAN_POINT('Ctrl Pts',(198.804855333026,98.4647380908065,341.729331481144));
#25315=CARTESIAN_POINT('Ctrl Pts',(197.704812491401,98.4022380908064,339.974558257745));
#25316=CARTESIAN_POINT('Ctrl Pts',(198.167776784202,98.3397380908064,337.955898459125));
#25317=CARTESIAN_POINT('Ctrl Pts',(198.630741077004,98.2772380908064,335.937238660506));
#25318=CARTESIAN_POINT('Ctrl Pts',(200.385514300403,98.2147380908065,334.837195818881));
#25319=CARTESIAN_POINT('Ctrl Pts',(202.140287523803,98.1522380908065,333.737152977255));
#25320=CARTESIAN_POINT('Ctrl Pts',(204.158947322422,98.0897380908065,334.200117270057));
#25321=CARTESIAN_POINT('Ctrl Pts',(206.177607121041,98.0272380908065,334.663081562858));
#25322=CARTESIAN_POINT('Ctrl Pts',(207.277649962667,97.9647380908064,336.417854786258));
#25323=CARTESIAN_POINT('Ctrl Pts',(208.377692804292,97.9022380908064,338.172628009657));
#25324=CARTESIAN_POINT('Ctrl Pts',(207.914728511491,97.8397380908065,340.191287808277));
#25325=CARTESIAN_POINT('Ctrl Pts',(207.451764218689,97.7772380908064,342.209947606896));
#25326=CARTESIAN_POINT('Ctrl Pts',(205.69699099529,97.7147380908064,343.309990448521));
#25327=CARTESIAN_POINT('Ctrl Pts',(203.94221777189,97.6522380908065,344.410033290147));
#25328=CARTESIAN_POINT('Ctrl Pts',(201.923557973271,97.5897380908064,343.947068997345));
#25329=CARTESIAN_POINT('Ctrl Pts',(199.904898174651,97.5272380908065,343.484104704544));
#25330=CARTESIAN_POINT('Ctrl Pts',(198.804855333026,97.4647380908065,341.729331481144));
#25331=CARTESIAN_POINT('Ctrl Pts',(197.704812491401,97.4022380908064,339.974558257745));
#25332=CARTESIAN_POINT('Ctrl Pts',(198.167776784202,97.3397380908064,337.955898459125));
#25333=CARTESIAN_POINT('Ctrl Pts',(198.630741077004,97.2772380908065,335.937238660506));
#25334=CARTESIAN_POINT('Ctrl Pts',(200.385514300403,97.2147380908064,334.837195818881));
#25335=CARTESIAN_POINT('Ctrl Pts',(202.140287523803,97.1522380908065,333.737152977255));
#25336=CARTESIAN_POINT('Ctrl Pts',(204.158947322422,97.0897380908065,334.200117270057));
#25337=CARTESIAN_POINT('Ctrl Pts',(206.177607121041,97.0272380908065,334.663081562858));
#25338=CARTESIAN_POINT('Ctrl Pts',(207.277649962667,96.9647380908064,336.417854786258));
#25339=CARTESIAN_POINT('Ctrl Pts',(208.377692804292,96.9022380908064,338.172628009657));
#25340=CARTESIAN_POINT('Ctrl Pts',(207.914728511491,96.8397380908065,340.191287808277));
#25341=CARTESIAN_POINT('Ctrl Pts',(207.451764218689,96.7772380908065,342.209947606896));
#25342=CARTESIAN_POINT('Ctrl Pts',(205.69699099529,96.7147380908065,343.309990448521));
#25343=CARTESIAN_POINT('Ctrl Pts',(203.94221777189,96.6522380908065,344.410033290147));
#25344=CARTESIAN_POINT('Ctrl Pts',(201.923557973271,96.5897380908064,343.947068997345));
#25345=CARTESIAN_POINT('Ctrl Pts',(199.904898174651,96.5272380908065,343.484104704544));
#25346=CARTESIAN_POINT('Ctrl Pts',(198.804855333026,96.4647380908065,341.729331481144));
#25347=CARTESIAN_POINT('Ctrl Pts',(197.704812491401,96.4022380908064,339.974558257745));
#25348=CARTESIAN_POINT('Ctrl Pts',(198.167776784202,96.3397380908064,337.955898459125));
#25349=CARTESIAN_POINT('Ctrl Pts',(198.630741077004,96.2772380908065,335.937238660506));
#25350=CARTESIAN_POINT('Ctrl Pts',(200.385514300403,96.2147380908064,334.837195818881));
#25351=CARTESIAN_POINT('Ctrl Pts',(202.140287523803,96.1522380908065,333.737152977255));
#25352=CARTESIAN_POINT('Ctrl Pts',(204.158947322422,96.0897380908065,334.200117270057));
#25353=CARTESIAN_POINT('Ctrl Pts',(206.177607121041,96.0272380908064,334.663081562858));
#25354=CARTESIAN_POINT('Ctrl Pts',(207.277649962667,95.9647380908064,336.417854786258));
#25355=CARTESIAN_POINT('Ctrl Pts',(208.377692804292,95.9022380908064,338.172628009657));
#25356=CARTESIAN_POINT('Ctrl Pts',(207.914728511491,95.8397380908064,340.191287808277));
#25357=CARTESIAN_POINT('Ctrl Pts',(207.451764218689,95.7772380908065,342.209947606896));
#25358=CARTESIAN_POINT('Ctrl Pts',(205.69699099529,95.7147380908064,343.309990448521));
#25359=CARTESIAN_POINT('Ctrl Pts',(203.94221777189,95.6522380908065,344.410033290147));
#25360=CARTESIAN_POINT('Ctrl Pts',(201.923557973271,95.5897380908064,343.947068997345));
#25361=CARTESIAN_POINT('Ctrl Pts',(199.904898174651,95.5272380908064,343.484104704544));
#25362=CARTESIAN_POINT('Ctrl Pts',(198.804855333026,95.4647380908065,341.729331481144));
#25363=CARTESIAN_POINT('Ctrl Pts',(197.704812491401,95.4022380908064,339.974558257745));
#25364=CARTESIAN_POINT('Ctrl Pts',(198.167776784202,95.3397380908065,337.955898459125));
#25365=CARTESIAN_POINT('Ctrl Pts',(198.630741077004,95.2772380908065,335.937238660506));
#25366=CARTESIAN_POINT('Ctrl Pts',(200.385514300403,95.2147380908064,334.837195818881));
#25367=CARTESIAN_POINT('Ctrl Pts',(202.140287523803,95.1522380908065,333.737152977255));
#25368=CARTESIAN_POINT('Ctrl Pts',(204.158947322422,95.0897380908064,334.200117270057));
#25369=CARTESIAN_POINT('Ctrl Pts',(206.177607121041,95.0272380908064,334.663081562858));
#25370=CARTESIAN_POINT('Ctrl Pts',(207.277649962667,94.9647380908064,336.417854786258));
#25371=CARTESIAN_POINT('Ctrl Pts',(208.377692804292,94.9022380908064,338.172628009657));
#25372=CARTESIAN_POINT('Ctrl Pts',(207.914728511491,94.8397380908064,340.191287808277));
#25373=CARTESIAN_POINT('Ctrl Pts',(207.451764218689,94.7772380908064,342.209947606896));
#25374=CARTESIAN_POINT('Ctrl Pts',(205.69699099529,94.7147380908065,343.309990448521));
#25375=CARTESIAN_POINT('Ctrl Pts',(203.94221777189,94.6522380908065,344.410033290147));
#25376=CARTESIAN_POINT('Ctrl Pts',(201.923557973271,94.5897380908064,343.947068997345));
#25377=CARTESIAN_POINT('Ctrl Pts',(199.904898174651,94.5272380908064,343.484104704544));
#25378=CARTESIAN_POINT('Ctrl Pts',(198.804855333026,94.4647380908064,341.729331481144));
#25379=CARTESIAN_POINT('Ctrl Pts',(197.704812491401,94.4022380908064,339.974558257745));
#25380=CARTESIAN_POINT('Ctrl Pts',(198.167776784202,94.3397380908065,337.955898459125));
#25381=CARTESIAN_POINT('Ctrl Pts',(198.630741077004,94.2772380908064,335.937238660506));
#25382=CARTESIAN_POINT('Ctrl Pts',(200.385514300403,94.2147380908064,334.837195818881));
#25383=CARTESIAN_POINT('Ctrl Pts',(202.140287523803,94.1522380908065,333.737152977255));
#25384=CARTESIAN_POINT('Ctrl Pts',(204.158947322422,94.0897380908065,334.200117270057));
#25385=CARTESIAN_POINT('Ctrl Pts',(206.177607121041,94.0272380908064,334.663081562858));
#25386=CARTESIAN_POINT('Ctrl Pts',(207.277649962667,93.9647380908065,336.417854786258));
#25387=CARTESIAN_POINT('Ctrl Pts',(208.377692804292,93.9022380908064,338.172628009657));
#25388=CARTESIAN_POINT('Ctrl Pts',(207.914728511491,93.8397380908064,340.191287808277));
#25389=CARTESIAN_POINT('Ctrl Pts',(207.451764218689,93.7772380908065,342.209947606896));
#25390=CARTESIAN_POINT('Ctrl Pts',(205.69699099529,93.7147380908065,343.309990448521));
#25391=CARTESIAN_POINT('Ctrl Pts',(203.94221777189,93.6522380908064,344.410033290147));
#25392=CARTESIAN_POINT('Ctrl Pts',(201.923557973271,93.5897380908064,343.947068997345));
#25393=CARTESIAN_POINT('Ctrl Pts',(199.904898174651,93.5272380908064,343.484104704544));
#25394=CARTESIAN_POINT('Ctrl Pts',(198.804855333026,93.4647380908064,341.729331481144));
#25395=CARTESIAN_POINT('Ctrl Pts',(197.704812491401,93.4022380908064,339.974558257745));
#25396=CARTESIAN_POINT('Ctrl Pts',(198.167776784202,93.3397380908065,337.955898459125));
#25397=CARTESIAN_POINT('Ctrl Pts',(198.630741077004,93.2772380908065,335.937238660506));
#25398=CARTESIAN_POINT('Ctrl Pts',(200.385514300403,93.2147380908064,334.837195818881));
#25399=CARTESIAN_POINT('Ctrl Pts',(202.140287523803,93.1522380908065,333.737152977255));
#25400=CARTESIAN_POINT('Ctrl Pts',(204.158947322422,93.0897380908064,334.200117270057));
#25401=CARTESIAN_POINT('Ctrl Pts',(206.177607121041,93.0272380908064,334.663081562858));
#25402=CARTESIAN_POINT('Ctrl Pts',(207.277649962667,92.9647380908065,336.417854786258));
#25403=CARTESIAN_POINT('Ctrl Pts',(208.377692804292,92.9022380908064,338.172628009657));
#25404=CARTESIAN_POINT('Ctrl Pts',(207.914728511491,92.8397380908064,340.191287808277));
#25405=CARTESIAN_POINT('Ctrl Pts',(207.451764218689,92.7772380908065,342.209947606896));
#25406=CARTESIAN_POINT('Ctrl Pts',(205.69699099529,92.7147380908065,343.309990448521));
#25407=CARTESIAN_POINT('Ctrl Pts',(203.94221777189,92.6522380908065,344.410033290147));
#25408=CARTESIAN_POINT('Ctrl Pts',(201.923557973271,92.5897380908064,343.947068997345));
#25409=CARTESIAN_POINT('Ctrl Pts',(199.904898174651,92.5272380908064,343.484104704544));
#25410=CARTESIAN_POINT('Ctrl Pts',(198.804855333026,92.4647380908064,341.729331481144));
#25411=CARTESIAN_POINT('Ctrl Pts',(197.704812491401,92.4022380908064,339.974558257745));
#25412=CARTESIAN_POINT('Ctrl Pts',(198.167776784202,92.3397380908065,337.955898459125));
#25413=CARTESIAN_POINT('Ctrl Pts',(198.630741077004,92.2772380908064,335.937238660506));
#25414=CARTESIAN_POINT('Ctrl Pts',(200.385514300403,92.2147380908064,334.837195818881));
#25415=CARTESIAN_POINT('Ctrl Pts',(202.140287523803,92.1522380908065,333.737152977255));
#25416=CARTESIAN_POINT('Ctrl Pts',(204.158947322422,92.0897380908064,334.200117270057));
#25417=CARTESIAN_POINT('Ctrl Pts',(206.177607121041,92.0272380908064,334.663081562858));
#25418=CARTESIAN_POINT('Ctrl Pts',(207.277649962667,91.9647380908064,336.417854786258));
#25419=CARTESIAN_POINT('Ctrl Pts',(208.377692804292,91.9022380908064,338.172628009657));
#25420=CARTESIAN_POINT('Ctrl Pts',(207.914728511491,91.8397380908064,340.191287808277));
#25421=CARTESIAN_POINT('Ctrl Pts',(207.451764218689,91.7772380908065,342.209947606896));
#25422=CARTESIAN_POINT('Ctrl Pts',(205.69699099529,91.7147380908064,343.309990448521));
#25423=CARTESIAN_POINT('Ctrl Pts',(203.94221777189,91.6522380908064,344.410033290147));
#25424=CARTESIAN_POINT('Ctrl Pts',(201.923557973271,91.5897380908064,343.947068997345));
#25425=CARTESIAN_POINT('Ctrl Pts',(199.904898174651,91.5272380908064,343.484104704544));
#25426=CARTESIAN_POINT('Ctrl Pts',(198.804855333026,91.4647380908064,341.729331481144));
#25427=CARTESIAN_POINT('Ctrl Pts',(197.704812491401,91.4022380908064,339.974558257745));
#25428=CARTESIAN_POINT('Ctrl Pts',(198.167776784202,91.3397380908064,337.955898459125));
#25429=CARTESIAN_POINT('Ctrl Pts',(198.630741077004,91.2772380908065,335.937238660506));
#25430=CARTESIAN_POINT('Ctrl Pts',(200.385514300403,91.2147380908064,334.837195818881));
#25431=CARTESIAN_POINT('Ctrl Pts',(202.140287523803,91.1522380908065,333.737152977255));
#25432=CARTESIAN_POINT('Ctrl Pts',(204.158947322422,91.0897380908064,334.200117270057));
#25433=CARTESIAN_POINT('Ctrl Pts',(206.177607121041,91.0272380908064,334.663081562858));
#25434=CARTESIAN_POINT('Ctrl Pts',(207.277649962667,90.9647380908065,336.417854786258));
#25435=CARTESIAN_POINT('Ctrl Pts',(208.377692804292,90.9022380908064,338.172628009657));
#25436=CARTESIAN_POINT('Ctrl Pts',(207.914728511491,90.8397380908064,340.191287808277));
#25437=CARTESIAN_POINT('Ctrl Pts',(207.451764218689,90.7772380908065,342.209947606896));
#25438=CARTESIAN_POINT('Ctrl Pts',(205.69699099529,90.7147380908064,343.309990448521));
#25439=CARTESIAN_POINT('Ctrl Pts',(203.94221777189,90.6522380908064,344.410033290147));
#25440=CARTESIAN_POINT('Ctrl Pts',(201.923557973271,90.5897380908065,343.947068997345));
#25441=CARTESIAN_POINT('Ctrl Pts',(199.904898174651,90.5272380908064,343.484104704544));
#25442=CARTESIAN_POINT('Ctrl Pts',(198.804855333026,90.4647380908064,341.729331481144));
#25443=CARTESIAN_POINT('Ctrl Pts',(197.704812491401,90.4022380908064,339.974558257745));
#25444=CARTESIAN_POINT('Ctrl Pts',(198.167776784202,90.3397380908064,337.955898459125));
#25445=CARTESIAN_POINT('Ctrl Pts',(198.630741077004,90.2772380908065,335.937238660506));
#25446=CARTESIAN_POINT('Ctrl Pts',(200.385514300403,90.2147380908065,334.837195818881));
#25447=CARTESIAN_POINT('Ctrl Pts',(202.140287523803,90.1522380908065,333.737152977255));
#25448=CARTESIAN_POINT('Ctrl Pts',(204.158947322422,90.0897380908064,334.200117270057));
#25449=CARTESIAN_POINT('Ctrl Pts',(206.177607121041,90.0272380908064,334.663081562858));
#25450=CARTESIAN_POINT('Ctrl Pts',(207.277649962667,89.9647380908065,336.417854786258));
#25451=CARTESIAN_POINT('Ctrl Pts',(208.377692804292,89.9022380908064,338.172628009657));
#25452=CARTESIAN_POINT('Ctrl Pts',(207.914728511491,89.8397380908065,340.191287808277));
#25453=CARTESIAN_POINT('Ctrl Pts',(207.451764218689,89.7772380908064,342.209947606896));
#25454=CARTESIAN_POINT('Ctrl Pts',(205.69699099529,89.7147380908064,343.309990448521));
#25455=CARTESIAN_POINT('Ctrl Pts',(203.94221777189,89.6522380908064,344.410033290147));
#25456=CARTESIAN_POINT('Ctrl Pts',(201.923557973271,89.5897380908065,343.947068997345));
#25457=CARTESIAN_POINT('Ctrl Pts',(199.904898174651,89.5272380908064,343.484104704544));
#25458=CARTESIAN_POINT('Ctrl Pts',(198.804855333026,89.4647380908064,341.729331481144));
#25459=CARTESIAN_POINT('Ctrl Pts',(197.704812491401,89.4022380908064,339.974558257745));
#25460=CARTESIAN_POINT('Ctrl Pts',(198.167776784202,89.3397380908064,337.955898459125));
#25461=CARTESIAN_POINT('Ctrl Pts',(198.630741077004,89.2772380908065,335.937238660506));
#25462=CARTESIAN_POINT('Ctrl Pts',(200.385514300403,89.2147380908065,334.837195818881));
#25463=CARTESIAN_POINT('Ctrl Pts',(202.140287523803,89.1522380908064,333.737152977255));
#25464=CARTESIAN_POINT('Ctrl Pts',(204.158947322422,89.0897380908064,334.200117270057));
#25465=CARTESIAN_POINT('Ctrl Pts',(206.177607121041,89.0272380908065,334.663081562858));
#25466=CARTESIAN_POINT('Ctrl Pts',(207.277649962667,88.9647380908064,336.417854786258));
#25467=CARTESIAN_POINT('Ctrl Pts',(208.377692804292,88.9022380908065,338.172628009657));
#25468=CARTESIAN_POINT('Ctrl Pts',(207.914728511491,88.8397380908064,340.191287808277));
#25469=CARTESIAN_POINT('Ctrl Pts',(207.451764218689,88.7772380908064,342.209947606896));
#25470=CARTESIAN_POINT('Ctrl Pts',(205.69699099529,88.7147380908064,343.309990448521));
#25471=CARTESIAN_POINT('Ctrl Pts',(203.94221777189,88.6522380908064,344.410033290147));
#25472=CARTESIAN_POINT('Ctrl Pts',(201.923557973271,88.5897380908065,343.947068997345));
#25473=CARTESIAN_POINT('Ctrl Pts',(199.904898174651,88.5272380908064,343.484104704544));
#25474=CARTESIAN_POINT('Ctrl Pts',(198.804855333026,88.4647380908065,341.729331481144));
#25475=CARTESIAN_POINT('Ctrl Pts',(197.704812491401,88.4022380908065,339.974558257745));
#25476=CARTESIAN_POINT('Ctrl Pts',(198.167776784202,88.3397380908064,337.955898459125));
#25477=CARTESIAN_POINT('Ctrl Pts',(198.630741077004,88.2772380908065,335.937238660506));
#25478=CARTESIAN_POINT('Ctrl Pts',(200.385514300403,88.2147380908064,334.837195818881));
#25479=CARTESIAN_POINT('Ctrl Pts',(202.140287523803,88.1522380908064,333.737152977255));
#25480=CARTESIAN_POINT('Ctrl Pts',(204.158947322422,88.0897380908064,334.200117270057));
#25481=CARTESIAN_POINT('Ctrl Pts',(207.107563775619,100.631003482039,337.244543159099));
#25482=CARTESIAN_POINT('Ctrl Pts',(207.721960531643,100.577922561033,338.610459017374));
#25483=CARTESIAN_POINT('Ctrl Pts',(207.38715854767,100.527237608405,340.070293644044));
#25484=CARTESIAN_POINT('Ctrl Pts',(206.974311678662,100.464737608405,341.870426808548));
#25485=CARTESIAN_POINT('Ctrl Pts',(205.409498490334,100.402237608405,342.851386355541));
#25486=CARTESIAN_POINT('Ctrl Pts',(203.844685302007,100.339737608405,343.832345902533));
#25487=CARTESIAN_POINT('Ctrl Pts',(202.044552137503,100.277237608405,343.419499033524));
#25488=CARTESIAN_POINT('Origin',(203.041252647847,101.652237608405,339.0735931337));
#25489=CARTESIAN_POINT('Ctrl Pts',(201.212202673244,100.631003482039,335.007282005928));
#25490=CARTESIAN_POINT('Ctrl Pts',(202.578118531519,100.577922561033,334.392885249905));
#25491=CARTESIAN_POINT('Ctrl Pts',(204.03795315819,100.527237608405,334.727687233877));
#25492=CARTESIAN_POINT('Ctrl Pts',(205.838086322694,100.464737608405,335.140534102886));
#25493=CARTESIAN_POINT('Ctrl Pts',(206.819045869686,100.402237608405,336.705347291213));
#25494=CARTESIAN_POINT('Ctrl Pts',(207.800005416678,100.339737608405,338.27016047954));
#25495=CARTESIAN_POINT('Ctrl Pts',(207.38715854767,100.277237608405,340.070293644044));
#25496=CARTESIAN_POINT('Ctrl Pts',(206.974311678662,100.214737608405,341.870426808548));
#25497=CARTESIAN_POINT('Ctrl Pts',(205.409498490334,100.152237608405,342.851386355541));
#25498=CARTESIAN_POINT('Ctrl Pts',(203.844685302007,100.089737608405,343.832345902533));
#25499=CARTESIAN_POINT('Ctrl Pts',(202.044552137503,100.027237608405,343.419499033524));
#25500=CARTESIAN_POINT('Ctrl Pts',(204.158947135117,101.21473760977,334.200118086763));
#25501=CARTESIAN_POINT('Ctrl Pts',(206.177606595445,101.15223760977,334.66308230198));
#25502=CARTESIAN_POINT('Ctrl Pts',(207.277649252723,101.08973760977,336.417855231311));
#25503=CARTESIAN_POINT('Ctrl Pts',(208.377691910001,101.02723760977,338.172628160643));
#25504=CARTESIAN_POINT('Ctrl Pts',(207.914727694784,100.96473760977,340.191287620971));
#25505=CARTESIAN_POINT('Ctrl Pts',(207.451763479567,100.90223760977,342.2099470813));
#25506=CARTESIAN_POINT('Ctrl Pts',(205.696990550236,100.83973760977,343.309989738578));
#25507=CARTESIAN_POINT('Ctrl Pts',(203.942217620905,100.77723760977,344.410032395856));
#25508=CARTESIAN_POINT('Ctrl Pts',(201.923558160576,100.71473760977,343.947068180639));
#25509=CARTESIAN_POINT('Ctrl Pts',(199.904898700248,100.65223760977,343.484103965422));
#25510=CARTESIAN_POINT('Ctrl Pts',(198.80485604297,100.58973760977,341.72933103609));
#25511=CARTESIAN_POINT('Ctrl Pts',(197.704813385692,100.52723760977,339.974558106759));
#25512=CARTESIAN_POINT('Ctrl Pts',(198.167777600909,100.46473760977,337.955898646431));
#25513=CARTESIAN_POINT('Ctrl Pts',(198.630741816126,100.40223760977,335.937239186102));
#25514=CARTESIAN_POINT('Ctrl Pts',(200.385514745457,100.33973760977,334.837196528824));
#25515=CARTESIAN_POINT('Ctrl Pts',(202.140287674788,100.27723760977,333.737153871546));
#25516=CARTESIAN_POINT('Ctrl Pts',(204.158947135117,100.21473760977,334.200118086763));
#25517=CARTESIAN_POINT('Ctrl Pts',(206.177606595445,100.15223760977,334.66308230198));
#25518=CARTESIAN_POINT('Ctrl Pts',(207.277649252723,100.08973760977,336.417855231311));
#25519=CARTESIAN_POINT('Ctrl Pts',(208.377691910001,100.02723760977,338.172628160643));
#25520=CARTESIAN_POINT('Ctrl Pts',(207.914727694784,99.9647376097703,340.191287620971));
#25521=CARTESIAN_POINT('Ctrl Pts',(207.451763479567,99.9022376097703,342.2099470813));
#25522=CARTESIAN_POINT('Ctrl Pts',(205.696990550236,99.8397376097703,343.309989738578));
#25523=CARTESIAN_POINT('Ctrl Pts',(203.942217620905,99.7772376097703,344.410032395856));
#25524=CARTESIAN_POINT('Ctrl Pts',(201.923558160576,99.7147376097703,343.947068180639));
#25525=CARTESIAN_POINT('Ctrl Pts',(199.904898700248,99.6522376097703,343.484103965422));
#25526=CARTESIAN_POINT('Ctrl Pts',(198.80485604297,99.5897376097703,341.72933103609));
#25527=CARTESIAN_POINT('Ctrl Pts',(197.704813385692,99.5272376097703,339.974558106759));
#25528=CARTESIAN_POINT('Ctrl Pts',(198.167777600909,99.4647376097703,337.955898646431));
#25529=CARTESIAN_POINT('Ctrl Pts',(198.630741816126,99.4022376097703,335.937239186102));
#25530=CARTESIAN_POINT('Ctrl Pts',(200.385514745457,99.3397376097703,334.837196528824));
#25531=CARTESIAN_POINT('Ctrl Pts',(202.140287674788,99.2772376097703,333.737153871546));
#25532=CARTESIAN_POINT('Ctrl Pts',(204.158947135117,99.2147376097703,334.200118086763));
#25533=CARTESIAN_POINT('Ctrl Pts',(206.177606595445,99.1522376097703,334.66308230198));
#25534=CARTESIAN_POINT('Ctrl Pts',(207.277649252723,99.0897376097703,336.417855231311));
#25535=CARTESIAN_POINT('Ctrl Pts',(208.377691910001,99.0272376097703,338.172628160643));
#25536=CARTESIAN_POINT('Ctrl Pts',(207.914727694784,98.9647376097703,340.191287620971));
#25537=CARTESIAN_POINT('Ctrl Pts',(207.451763479567,98.9022376097703,342.2099470813));
#25538=CARTESIAN_POINT('Ctrl Pts',(205.696990550236,98.8397376097703,343.309989738578));
#25539=CARTESIAN_POINT('Ctrl Pts',(203.942217620905,98.7772376097703,344.410032395856));
#25540=CARTESIAN_POINT('Ctrl Pts',(201.923558160576,98.7147376097703,343.947068180639));
#25541=CARTESIAN_POINT('Ctrl Pts',(199.904898700248,98.6522376097703,343.484103965422));
#25542=CARTESIAN_POINT('Ctrl Pts',(198.80485604297,98.5897376097703,341.72933103609));
#25543=CARTESIAN_POINT('Ctrl Pts',(197.704813385692,98.5272376097703,339.974558106759));
#25544=CARTESIAN_POINT('Ctrl Pts',(198.167777600909,98.4647376097703,337.955898646431));
#25545=CARTESIAN_POINT('Ctrl Pts',(198.630741816126,98.4022376097703,335.937239186102));
#25546=CARTESIAN_POINT('Ctrl Pts',(200.385514745457,98.3397376097703,334.837196528824));
#25547=CARTESIAN_POINT('Ctrl Pts',(202.140287674788,98.2772376097703,333.737153871546));
#25548=CARTESIAN_POINT('Ctrl Pts',(204.158947135117,98.2147376097703,334.200118086763));
#25549=CARTESIAN_POINT('Ctrl Pts',(206.177606595445,98.1522376097703,334.66308230198));
#25550=CARTESIAN_POINT('Ctrl Pts',(207.277649252723,98.0897376097703,336.417855231311));
#25551=CARTESIAN_POINT('Ctrl Pts',(208.377691910001,98.0272376097703,338.172628160643));
#25552=CARTESIAN_POINT('Ctrl Pts',(207.914727694784,97.9647376097703,340.191287620971));
#25553=CARTESIAN_POINT('Ctrl Pts',(207.451763479567,97.9022376097703,342.2099470813));
#25554=CARTESIAN_POINT('Ctrl Pts',(205.696990550236,97.8397376097703,343.309989738578));
#25555=CARTESIAN_POINT('Ctrl Pts',(203.942217620905,97.7772376097703,344.410032395856));
#25556=CARTESIAN_POINT('Ctrl Pts',(201.923558160576,97.7147376097703,343.947068180639));
#25557=CARTESIAN_POINT('Ctrl Pts',(199.904898700248,97.6522376097703,343.484103965422));
#25558=CARTESIAN_POINT('Ctrl Pts',(198.80485604297,97.5897376097703,341.72933103609));
#25559=CARTESIAN_POINT('Ctrl Pts',(197.704813385692,97.5272376097703,339.974558106759));
#25560=CARTESIAN_POINT('Ctrl Pts',(198.167777600909,97.4647376097703,337.955898646431));
#25561=CARTESIAN_POINT('Ctrl Pts',(198.630741816126,97.4022376097703,335.937239186102));
#25562=CARTESIAN_POINT('Ctrl Pts',(200.385514745457,97.3397376097703,334.837196528824));
#25563=CARTESIAN_POINT('Ctrl Pts',(202.140287674788,97.2772376097703,333.737153871546));
#25564=CARTESIAN_POINT('Ctrl Pts',(204.158947135117,97.2147376097703,334.200118086763));
#25565=CARTESIAN_POINT('Ctrl Pts',(206.177606595445,97.1522376097703,334.66308230198));
#25566=CARTESIAN_POINT('Ctrl Pts',(207.277649252723,97.0897376097703,336.417855231311));
#25567=CARTESIAN_POINT('Ctrl Pts',(208.377691910001,97.0272376097703,338.172628160643));
#25568=CARTESIAN_POINT('Ctrl Pts',(207.914727694784,96.9647376097703,340.191287620971));
#25569=CARTESIAN_POINT('Ctrl Pts',(207.451763479567,96.9022376097703,342.2099470813));
#25570=CARTESIAN_POINT('Ctrl Pts',(205.696990550236,96.8397376097703,343.309989738578));
#25571=CARTESIAN_POINT('Ctrl Pts',(203.942217620905,96.7772376097703,344.410032395856));
#25572=CARTESIAN_POINT('Ctrl Pts',(201.923558160576,96.7147376097703,343.947068180639));
#25573=CARTESIAN_POINT('Ctrl Pts',(199.904898700248,96.6522376097703,343.484103965422));
#25574=CARTESIAN_POINT('Ctrl Pts',(198.80485604297,96.5897376097703,341.72933103609));
#25575=CARTESIAN_POINT('Ctrl Pts',(197.704813385692,96.5272376097703,339.974558106759));
#25576=CARTESIAN_POINT('Ctrl Pts',(198.167777600909,96.4647376097703,337.955898646431));
#25577=CARTESIAN_POINT('Ctrl Pts',(198.630741816126,96.4022376097703,335.937239186102));
#25578=CARTESIAN_POINT('Ctrl Pts',(200.385514745457,96.3397376097703,334.837196528824));
#25579=CARTESIAN_POINT('Ctrl Pts',(202.140287674788,96.2772376097703,333.737153871546));
#25580=CARTESIAN_POINT('Ctrl Pts',(204.158947135117,96.2147376097703,334.200118086763));
#25581=CARTESIAN_POINT('Ctrl Pts',(206.177606595445,96.1522376097703,334.66308230198));
#25582=CARTESIAN_POINT('Ctrl Pts',(207.277649252723,96.0897376097703,336.417855231311));
#25583=CARTESIAN_POINT('Ctrl Pts',(208.377691910001,96.0272376097703,338.172628160643));
#25584=CARTESIAN_POINT('Ctrl Pts',(207.914727694784,95.9647376097703,340.191287620971));
#25585=CARTESIAN_POINT('Ctrl Pts',(207.451763479567,95.9022376097703,342.2099470813));
#25586=CARTESIAN_POINT('Ctrl Pts',(205.696990550236,95.8397376097703,343.309989738578));
#25587=CARTESIAN_POINT('Ctrl Pts',(203.942217620905,95.7772376097703,344.410032395856));
#25588=CARTESIAN_POINT('Ctrl Pts',(201.923558160576,95.7147376097703,343.947068180639));
#25589=CARTESIAN_POINT('Ctrl Pts',(199.904898700248,95.6522376097703,343.484103965422));
#25590=CARTESIAN_POINT('Ctrl Pts',(198.80485604297,95.5897376097703,341.72933103609));
#25591=CARTESIAN_POINT('Ctrl Pts',(197.704813385692,95.5272376097703,339.974558106759));
#25592=CARTESIAN_POINT('Ctrl Pts',(198.167777600909,95.4647376097703,337.955898646431));
#25593=CARTESIAN_POINT('Ctrl Pts',(198.630741816126,95.4022376097703,335.937239186102));
#25594=CARTESIAN_POINT('Ctrl Pts',(200.385514745457,95.3397376097703,334.837196528824));
#25595=CARTESIAN_POINT('Ctrl Pts',(202.140287674788,95.2772376097703,333.737153871546));
#25596=CARTESIAN_POINT('Ctrl Pts',(204.158947135117,95.2147376097703,334.200118086763));
#25597=CARTESIAN_POINT('Ctrl Pts',(206.177606595445,95.1522376097703,334.66308230198));
#25598=CARTESIAN_POINT('Ctrl Pts',(207.277649252723,95.0897376097703,336.417855231311));
#25599=CARTESIAN_POINT('Ctrl Pts',(208.377691910001,95.0272376097703,338.172628160643));
#25600=CARTESIAN_POINT('Ctrl Pts',(207.914727694784,94.9647376097703,340.191287620971));
#25601=CARTESIAN_POINT('Ctrl Pts',(207.451763479567,94.9022376097703,342.2099470813));
#25602=CARTESIAN_POINT('Ctrl Pts',(205.696990550236,94.8397376097703,343.309989738578));
#25603=CARTESIAN_POINT('Ctrl Pts',(203.942217620905,94.7772376097703,344.410032395856));
#25604=CARTESIAN_POINT('Ctrl Pts',(201.923558160576,94.7147376097703,343.947068180639));
#25605=CARTESIAN_POINT('Ctrl Pts',(199.904898700248,94.6522376097703,343.484103965422));
#25606=CARTESIAN_POINT('Ctrl Pts',(198.80485604297,94.5897376097703,341.72933103609));
#25607=CARTESIAN_POINT('Ctrl Pts',(197.704813385692,94.5272376097703,339.974558106759));
#25608=CARTESIAN_POINT('Ctrl Pts',(198.167777600909,94.4647376097703,337.955898646431));
#25609=CARTESIAN_POINT('Ctrl Pts',(198.630741816126,94.4022376097703,335.937239186102));
#25610=CARTESIAN_POINT('Ctrl Pts',(200.385514745457,94.3397376097703,334.837196528824));
#25611=CARTESIAN_POINT('Ctrl Pts',(202.140287674788,94.2772376097703,333.737153871546));
#25612=CARTESIAN_POINT('Ctrl Pts',(204.158947135117,94.2147376097703,334.200118086763));
#25613=CARTESIAN_POINT('Ctrl Pts',(206.177606595445,94.1522376097703,334.66308230198));
#25614=CARTESIAN_POINT('Ctrl Pts',(207.277649252723,94.0897376097703,336.417855231311));
#25615=CARTESIAN_POINT('Ctrl Pts',(208.377691910001,94.0272376097703,338.172628160643));
#25616=CARTESIAN_POINT('Ctrl Pts',(207.914727694784,93.9647376097703,340.191287620971));
#25617=CARTESIAN_POINT('Ctrl Pts',(207.451763479567,93.9022376097703,342.2099470813));
#25618=CARTESIAN_POINT('Ctrl Pts',(205.696990550236,93.8397376097703,343.309989738578));
#25619=CARTESIAN_POINT('Ctrl Pts',(203.942217620905,93.7772376097703,344.410032395856));
#25620=CARTESIAN_POINT('Ctrl Pts',(201.923558160576,93.7147376097703,343.947068180639));
#25621=CARTESIAN_POINT('Ctrl Pts',(199.904898700248,93.6522376097703,343.484103965422));
#25622=CARTESIAN_POINT('Ctrl Pts',(198.80485604297,93.5897376097703,341.72933103609));
#25623=CARTESIAN_POINT('Ctrl Pts',(197.704813385692,93.5272376097703,339.974558106759));
#25624=CARTESIAN_POINT('Ctrl Pts',(198.167777600909,93.4647376097703,337.955898646431));
#25625=CARTESIAN_POINT('Ctrl Pts',(198.630741816126,93.4022376097703,335.937239186102));
#25626=CARTESIAN_POINT('Ctrl Pts',(200.385514745457,93.3397376097703,334.837196528824));
#25627=CARTESIAN_POINT('Ctrl Pts',(202.140287674788,93.2772376097703,333.737153871546));
#25628=CARTESIAN_POINT('Ctrl Pts',(204.158947135117,93.2147376097703,334.200118086763));
#25629=CARTESIAN_POINT('Ctrl Pts',(206.177606595445,93.1522376097703,334.66308230198));
#25630=CARTESIAN_POINT('Ctrl Pts',(207.277649252723,93.0897376097703,336.417855231311));
#25631=CARTESIAN_POINT('Ctrl Pts',(208.377691910001,93.0272376097703,338.172628160643));
#25632=CARTESIAN_POINT('Ctrl Pts',(207.914727694784,92.9647376097703,340.191287620971));
#25633=CARTESIAN_POINT('Ctrl Pts',(207.451763479567,92.9022376097703,342.2099470813));
#25634=CARTESIAN_POINT('Ctrl Pts',(205.696990550236,92.8397376097703,343.309989738578));
#25635=CARTESIAN_POINT('Ctrl Pts',(203.942217620905,92.7772376097703,344.410032395856));
#25636=CARTESIAN_POINT('Ctrl Pts',(201.923558160576,92.7147376097703,343.947068180639));
#25637=CARTESIAN_POINT('Ctrl Pts',(199.904898700248,92.6522376097703,343.484103965422));
#25638=CARTESIAN_POINT('Ctrl Pts',(198.80485604297,92.5897376097703,341.72933103609));
#25639=CARTESIAN_POINT('Ctrl Pts',(197.704813385692,92.5272376097703,339.974558106759));
#25640=CARTESIAN_POINT('Ctrl Pts',(198.167777600909,92.4647376097703,337.955898646431));
#25641=CARTESIAN_POINT('Ctrl Pts',(198.630741816126,92.4022376097703,335.937239186102));
#25642=CARTESIAN_POINT('Ctrl Pts',(200.385514745457,92.3397376097703,334.837196528824));
#25643=CARTESIAN_POINT('Ctrl Pts',(202.140287674788,92.2772376097703,333.737153871546));
#25644=CARTESIAN_POINT('Ctrl Pts',(204.158947135117,92.2147376097703,334.200118086763));
#25645=CARTESIAN_POINT('Ctrl Pts',(206.177606595445,92.1522376097703,334.66308230198));
#25646=CARTESIAN_POINT('Ctrl Pts',(207.277649252723,92.0897376097703,336.417855231311));
#25647=CARTESIAN_POINT('Ctrl Pts',(208.377691910001,92.0272376097703,338.172628160643));
#25648=CARTESIAN_POINT('Ctrl Pts',(207.914727694784,91.9647376097703,340.191287620971));
#25649=CARTESIAN_POINT('Ctrl Pts',(207.451763479567,91.9022376097703,342.2099470813));
#25650=CARTESIAN_POINT('Ctrl Pts',(205.696990550236,91.8397376097703,343.309989738578));
#25651=CARTESIAN_POINT('Ctrl Pts',(203.942217620905,91.7772376097703,344.410032395856));
#25652=CARTESIAN_POINT('Ctrl Pts',(201.923558160576,91.7147376097703,343.947068180639));
#25653=CARTESIAN_POINT('Ctrl Pts',(199.904898700248,91.6522376097703,343.484103965422));
#25654=CARTESIAN_POINT('Ctrl Pts',(198.80485604297,91.5897376097703,341.72933103609));
#25655=CARTESIAN_POINT('Ctrl Pts',(197.704813385692,91.5272376097703,339.974558106759));
#25656=CARTESIAN_POINT('Ctrl Pts',(198.167777600909,91.4647376097703,337.955898646431));
#25657=CARTESIAN_POINT('Ctrl Pts',(198.630741816126,91.4022376097703,335.937239186102));
#25658=CARTESIAN_POINT('Ctrl Pts',(200.385514745457,91.3397376097703,334.837196528824));
#25659=CARTESIAN_POINT('Ctrl Pts',(202.140287674788,91.2772376097703,333.737153871546));
#25660=CARTESIAN_POINT('Ctrl Pts',(204.158947135117,91.2147376097703,334.200118086763));
#25661=CARTESIAN_POINT('Ctrl Pts',(206.177606595445,91.1522376097703,334.66308230198));
#25662=CARTESIAN_POINT('Ctrl Pts',(207.277649252723,91.0897376097703,336.417855231311));
#25663=CARTESIAN_POINT('Ctrl Pts',(208.377691910001,91.0272376097703,338.172628160643));
#25664=CARTESIAN_POINT('Ctrl Pts',(207.914727694784,90.9647376097703,340.191287620971));
#25665=CARTESIAN_POINT('Ctrl Pts',(207.451763479567,90.9022376097703,342.2099470813));
#25666=CARTESIAN_POINT('Ctrl Pts',(205.696990550236,90.8397376097703,343.309989738578));
#25667=CARTESIAN_POINT('Ctrl Pts',(203.942217620905,90.7772376097703,344.410032395856));
#25668=CARTESIAN_POINT('Ctrl Pts',(201.923558160576,90.7147376097703,343.947068180639));
#25669=CARTESIAN_POINT('Ctrl Pts',(199.904898700248,90.6522376097703,343.484103965422));
#25670=CARTESIAN_POINT('Ctrl Pts',(198.80485604297,90.5897376097703,341.72933103609));
#25671=CARTESIAN_POINT('Ctrl Pts',(197.704813385692,90.5272376097703,339.974558106759));
#25672=CARTESIAN_POINT('Ctrl Pts',(198.167777600909,90.4647376097703,337.955898646431));
#25673=CARTESIAN_POINT('Ctrl Pts',(198.630741816126,90.4022376097703,335.937239186102));
#25674=CARTESIAN_POINT('Ctrl Pts',(200.385514745457,90.3397376097703,334.837196528824));
#25675=CARTESIAN_POINT('Ctrl Pts',(202.140287674788,90.2772376097703,333.737153871546));
#25676=CARTESIAN_POINT('Ctrl Pts',(204.158947135117,90.2147376097703,334.200118086763));
#25677=CARTESIAN_POINT('Ctrl Pts',(206.177606595445,90.1522376097703,334.66308230198));
#25678=CARTESIAN_POINT('Ctrl Pts',(207.277649252723,90.0897376097703,336.417855231311));
#25679=CARTESIAN_POINT('Ctrl Pts',(208.377691910001,90.0272376097703,338.172628160643));
#25680=CARTESIAN_POINT('Ctrl Pts',(207.914727694784,89.9647376097703,340.191287620971));
#25681=CARTESIAN_POINT('Ctrl Pts',(207.451763479567,89.9022376097703,342.2099470813));
#25682=CARTESIAN_POINT('Ctrl Pts',(205.696990550236,89.8397376097703,343.309989738578));
#25683=CARTESIAN_POINT('Ctrl Pts',(203.942217620905,89.7772376097703,344.410032395856));
#25684=CARTESIAN_POINT('Ctrl Pts',(201.923558160576,89.7147376097703,343.947068180639));
#25685=CARTESIAN_POINT('Ctrl Pts',(199.904898700248,89.6522376097703,343.484103965422));
#25686=CARTESIAN_POINT('Ctrl Pts',(198.80485604297,89.5897376097703,341.72933103609));
#25687=CARTESIAN_POINT('Ctrl Pts',(197.704813385692,89.5272376097703,339.974558106759));
#25688=CARTESIAN_POINT('Ctrl Pts',(198.167777600909,89.4647376097703,337.955898646431));
#25689=CARTESIAN_POINT('Ctrl Pts',(198.630741816126,89.4022376097703,335.937239186102));
#25690=CARTESIAN_POINT('Ctrl Pts',(200.385514745457,89.3397376097703,334.837196528824));
#25691=CARTESIAN_POINT('Ctrl Pts',(202.140287674788,89.2772376097703,333.737153871546));
#25692=CARTESIAN_POINT('Ctrl Pts',(204.158947135117,89.2147376097703,334.200118086763));
#25693=CARTESIAN_POINT('Ctrl Pts',(206.177606595445,89.1522376097703,334.66308230198));
#25694=CARTESIAN_POINT('Ctrl Pts',(207.277649252723,89.0897376097703,336.417855231311));
#25695=CARTESIAN_POINT('Ctrl Pts',(208.377691910001,89.0272376097703,338.172628160643));
#25696=CARTESIAN_POINT('Ctrl Pts',(207.914727694784,88.9647376097703,340.191287620971));
#25697=CARTESIAN_POINT('Ctrl Pts',(207.451763479567,88.9022376097703,342.2099470813));
#25698=CARTESIAN_POINT('Ctrl Pts',(205.696990550236,88.8397376097703,343.309989738578));
#25699=CARTESIAN_POINT('Ctrl Pts',(203.942217620905,88.7772376097703,344.410032395856));
#25700=CARTESIAN_POINT('Ctrl Pts',(201.923558160576,88.7147376097703,343.947068180639));
#25701=CARTESIAN_POINT('Ctrl Pts',(199.904898700248,88.6522376097703,343.484103965422));
#25702=CARTESIAN_POINT('Ctrl Pts',(198.80485604297,88.5897376097703,341.72933103609));
#25703=CARTESIAN_POINT('Ctrl Pts',(197.704813385692,88.5272376097703,339.974558106759));
#25704=CARTESIAN_POINT('Ctrl Pts',(198.167777600909,88.4647376097703,337.955898646431));
#25705=CARTESIAN_POINT('Ctrl Pts',(198.630741816126,88.4022376097703,335.937239186102));
#25706=CARTESIAN_POINT('Ctrl Pts',(200.385514745457,88.3397376097703,334.837196528824));
#25707=CARTESIAN_POINT('Ctrl Pts',(202.140287674788,88.2772376097703,333.737153871546));
#25708=CARTESIAN_POINT('Ctrl Pts',(204.158947135117,88.2147376097703,334.200118086763));
#25709=CARTESIAN_POINT('Ctrl Pts',(206.177606595445,88.1522376097703,334.66308230198));
#25710=CARTESIAN_POINT('Ctrl Pts',(207.277649252723,88.0897376097703,336.417855231311));
#25711=CARTESIAN_POINT('Ctrl Pts',(208.377691910001,88.0272376097703,338.172628160643));
#25712=CARTESIAN_POINT('Ctrl Pts',(207.914727694784,87.9647376097703,340.191287620971));
#25713=CARTESIAN_POINT('Ctrl Pts',(207.451763479567,87.9022376097703,342.2099470813));
#25714=CARTESIAN_POINT('Ctrl Pts',(205.696990550236,87.8397376097703,343.309989738578));
#25715=CARTESIAN_POINT('Ctrl Pts',(203.942217620905,87.7772376097703,344.410032395856));
#25716=CARTESIAN_POINT('Ctrl Pts',(201.923558160576,87.7147376097703,343.947068180639));
#25717=CARTESIAN_POINT('Ctrl Pts',(199.904898700248,87.6522376097703,343.484103965422));
#25718=CARTESIAN_POINT('Ctrl Pts',(198.80485604297,87.5897376097703,341.72933103609));
#25719=CARTESIAN_POINT('Ctrl Pts',(197.704813385692,87.5272376097703,339.974558106759));
#25720=CARTESIAN_POINT('Ctrl Pts',(198.167777600909,87.4647376097703,337.955898646431));
#25721=CARTESIAN_POINT('Ctrl Pts',(198.630741816126,87.4022376097703,335.937239186102));
#25722=CARTESIAN_POINT('Ctrl Pts',(200.385514745457,87.3397376097703,334.837196528824));
#25723=CARTESIAN_POINT('Ctrl Pts',(202.140287674788,87.2772376097703,333.737153871546));
#25724=CARTESIAN_POINT('Ctrl Pts',(204.158947135117,87.2147376097703,334.200118086763));
#25725=CARTESIAN_POINT('Ctrl Pts',(204.03795315819,101.527237608405,334.727687233877));
#25726=CARTESIAN_POINT('Ctrl Pts',(205.838086322694,101.464737608405,335.140534102886));
#25727=CARTESIAN_POINT('Ctrl Pts',(206.819045869686,101.402237608405,336.705347291213));
#25728=CARTESIAN_POINT('Ctrl Pts',(207.800005416678,101.339737608405,338.27016047954));
#25729=CARTESIAN_POINT('Ctrl Pts',(207.38715854767,101.277237608405,340.070293644044));
#25730=CARTESIAN_POINT('Ctrl Pts',(206.974311678662,101.214737608405,341.870426808548));
#25731=CARTESIAN_POINT('Ctrl Pts',(205.409498490334,101.152237608405,342.851386355541));
#25732=CARTESIAN_POINT('Ctrl Pts',(203.844685302007,101.089737608405,343.832345902533));
#25733=CARTESIAN_POINT('Ctrl Pts',(202.044552137503,101.027237608405,343.419499033524));
#25734=CARTESIAN_POINT('Ctrl Pts',(200.244418972999,100.964737608405,343.006652164516));
#25735=CARTESIAN_POINT('Ctrl Pts',(199.263459426007,100.902237608405,341.441838976189));
#25736=CARTESIAN_POINT('Ctrl Pts',(198.282499879015,100.839737608405,339.877025787862));
#25737=CARTESIAN_POINT('Ctrl Pts',(198.695346748023,100.777237608405,338.076892623358));
#25738=CARTESIAN_POINT('Ctrl Pts',(199.108193617031,100.714737608405,336.276759458854));
#25739=CARTESIAN_POINT('Ctrl Pts',(200.673006805358,100.652237608405,335.295799911861));
#25740=CARTESIAN_POINT('Ctrl Pts',(202.237819993686,100.589737608405,334.314840364869));
#25741=CARTESIAN_POINT('Ctrl Pts',(204.03795315819,100.527237608405,334.727687233877));
#25742=CARTESIAN_POINT('Ctrl Pts',(205.838086322694,100.464737608405,335.140534102886));
#25743=CARTESIAN_POINT('Ctrl Pts',(206.819045869686,100.402237608405,336.705347291213));
#25744=CARTESIAN_POINT('Ctrl Pts',(207.800005416678,100.339737608405,338.27016047954));
#25745=CARTESIAN_POINT('Ctrl Pts',(207.38715854767,100.277237608405,340.070293644044));
#25746=CARTESIAN_POINT('Ctrl Pts',(206.974311678662,100.214737608405,341.870426808548));
#25747=CARTESIAN_POINT('Ctrl Pts',(205.409498490334,100.152237608405,342.851386355541));
#25748=CARTESIAN_POINT('Ctrl Pts',(203.844685302007,100.089737608405,343.832345902533));
#25749=CARTESIAN_POINT('Ctrl Pts',(202.044552137503,100.027237608405,343.419499033524));
#25750=CARTESIAN_POINT('Ctrl Pts',(200.244418972999,99.9647376084047,343.006652164516));
#25751=CARTESIAN_POINT('Ctrl Pts',(199.263459426007,99.9022376084047,341.441838976189));
#25752=CARTESIAN_POINT('Ctrl Pts',(198.282499879015,99.8397376084047,339.877025787862));
#25753=CARTESIAN_POINT('Ctrl Pts',(198.695346748023,99.7772376084047,338.076892623358));
#25754=CARTESIAN_POINT('Ctrl Pts',(199.108193617031,99.7147376084047,336.276759458854));
#25755=CARTESIAN_POINT('Ctrl Pts',(200.673006805358,99.6522376084047,335.295799911861));
#25756=CARTESIAN_POINT('Ctrl Pts',(202.237819993686,99.5897376084047,334.314840364869));
#25757=CARTESIAN_POINT('Ctrl Pts',(204.03795315819,99.5272376084047,334.727687233877));
#25758=CARTESIAN_POINT('Ctrl Pts',(205.838086322694,99.4647376084047,335.140534102886));
#25759=CARTESIAN_POINT('Ctrl Pts',(206.819045869686,99.4022376084047,336.705347291213));
#25760=CARTESIAN_POINT('Ctrl Pts',(207.800005416678,99.3397376084047,338.27016047954));
#25761=CARTESIAN_POINT('Ctrl Pts',(207.38715854767,99.2772376084047,340.070293644044));
#25762=CARTESIAN_POINT('Ctrl Pts',(206.974311678662,99.2147376084047,341.870426808548));
#25763=CARTESIAN_POINT('Ctrl Pts',(205.409498490334,99.1522376084047,342.851386355541));
#25764=CARTESIAN_POINT('Ctrl Pts',(203.844685302007,99.0897376084047,343.832345902533));
#25765=CARTESIAN_POINT('Ctrl Pts',(202.044552137503,99.0272376084047,343.419499033524));
#25766=CARTESIAN_POINT('Ctrl Pts',(200.244418972999,98.9647376084047,343.006652164516));
#25767=CARTESIAN_POINT('Ctrl Pts',(199.263459426007,98.9022376084047,341.441838976189));
#25768=CARTESIAN_POINT('Ctrl Pts',(198.282499879015,98.8397376084047,339.877025787862));
#25769=CARTESIAN_POINT('Ctrl Pts',(198.695346748023,98.7772376084047,338.076892623358));
#25770=CARTESIAN_POINT('Ctrl Pts',(199.108193617031,98.7147376084047,336.276759458854));
#25771=CARTESIAN_POINT('Ctrl Pts',(200.673006805358,98.6522376084047,335.295799911861));
#25772=CARTESIAN_POINT('Ctrl Pts',(202.237819993686,98.5897376084047,334.314840364869));
#25773=CARTESIAN_POINT('Ctrl Pts',(204.03795315819,98.5272376084047,334.727687233877));
#25774=CARTESIAN_POINT('Ctrl Pts',(205.838086322694,98.4647376084047,335.140534102886));
#25775=CARTESIAN_POINT('Ctrl Pts',(206.819045869686,98.4022376084047,336.705347291213));
#25776=CARTESIAN_POINT('Ctrl Pts',(207.800005416678,98.3397376084047,338.27016047954));
#25777=CARTESIAN_POINT('Ctrl Pts',(207.38715854767,98.2772376084047,340.070293644044));
#25778=CARTESIAN_POINT('Ctrl Pts',(206.974311678662,98.2147376084047,341.870426808548));
#25779=CARTESIAN_POINT('Ctrl Pts',(205.409498490334,98.1522376084047,342.851386355541));
#25780=CARTESIAN_POINT('Ctrl Pts',(203.844685302007,98.0897376084047,343.832345902533));
#25781=CARTESIAN_POINT('Ctrl Pts',(202.044552137503,98.0272376084047,343.419499033524));
#25782=CARTESIAN_POINT('Ctrl Pts',(200.244418972999,97.9647376084047,343.006652164516));
#25783=CARTESIAN_POINT('Ctrl Pts',(199.263459426007,97.9022376084047,341.441838976189));
#25784=CARTESIAN_POINT('Ctrl Pts',(198.282499879015,97.8397376084047,339.877025787862));
#25785=CARTESIAN_POINT('Ctrl Pts',(198.695346748023,97.7772376084047,338.076892623358));
#25786=CARTESIAN_POINT('Ctrl Pts',(199.108193617031,97.7147376084047,336.276759458854));
#25787=CARTESIAN_POINT('Ctrl Pts',(200.673006805358,97.6522376084047,335.295799911861));
#25788=CARTESIAN_POINT('Ctrl Pts',(202.237819993686,97.5897376084047,334.314840364869));
#25789=CARTESIAN_POINT('Ctrl Pts',(204.03795315819,97.5272376084047,334.727687233877));
#25790=CARTESIAN_POINT('Ctrl Pts',(205.838086322694,97.4647376084047,335.140534102886));
#25791=CARTESIAN_POINT('Ctrl Pts',(206.819045869686,97.4022376084047,336.705347291213));
#25792=CARTESIAN_POINT('Ctrl Pts',(207.800005416678,97.3397376084047,338.27016047954));
#25793=CARTESIAN_POINT('Ctrl Pts',(207.38715854767,97.2772376084047,340.070293644044));
#25794=CARTESIAN_POINT('Ctrl Pts',(206.974311678662,97.2147376084047,341.870426808548));
#25795=CARTESIAN_POINT('Ctrl Pts',(205.409498490334,97.1522376084047,342.851386355541));
#25796=CARTESIAN_POINT('Ctrl Pts',(203.844685302007,97.0897376084047,343.832345902533));
#25797=CARTESIAN_POINT('Ctrl Pts',(202.044552137503,97.0272376084047,343.419499033524));
#25798=CARTESIAN_POINT('Ctrl Pts',(200.244418972999,96.9647376084047,343.006652164516));
#25799=CARTESIAN_POINT('Ctrl Pts',(199.263459426007,96.9022376084047,341.441838976189));
#25800=CARTESIAN_POINT('Ctrl Pts',(198.282499879015,96.8397376084047,339.877025787862));
#25801=CARTESIAN_POINT('Ctrl Pts',(198.695346748023,96.7772376084047,338.076892623358));
#25802=CARTESIAN_POINT('Ctrl Pts',(199.108193617031,96.7147376084047,336.276759458854));
#25803=CARTESIAN_POINT('Ctrl Pts',(200.673006805358,96.6522376084047,335.295799911861));
#25804=CARTESIAN_POINT('Ctrl Pts',(202.237819993686,96.5897376084047,334.314840364869));
#25805=CARTESIAN_POINT('Ctrl Pts',(204.03795315819,96.5272376084047,334.727687233877));
#25806=CARTESIAN_POINT('Ctrl Pts',(205.838086322694,96.4647376084047,335.140534102886));
#25807=CARTESIAN_POINT('Ctrl Pts',(206.819045869686,96.4022376084047,336.705347291213));
#25808=CARTESIAN_POINT('Ctrl Pts',(207.800005416678,96.3397376084047,338.27016047954));
#25809=CARTESIAN_POINT('Ctrl Pts',(207.38715854767,96.2772376084047,340.070293644044));
#25810=CARTESIAN_POINT('Ctrl Pts',(206.974311678662,96.2147376084047,341.870426808548));
#25811=CARTESIAN_POINT('Ctrl Pts',(205.409498490334,96.1522376084047,342.851386355541));
#25812=CARTESIAN_POINT('Ctrl Pts',(203.844685302007,96.0897376084047,343.832345902533));
#25813=CARTESIAN_POINT('Ctrl Pts',(202.044552137503,96.0272376084047,343.419499033524));
#25814=CARTESIAN_POINT('Ctrl Pts',(200.244418972999,95.9647376084047,343.006652164516));
#25815=CARTESIAN_POINT('Ctrl Pts',(199.263459426007,95.9022376084047,341.441838976189));
#25816=CARTESIAN_POINT('Ctrl Pts',(198.282499879015,95.8397376084047,339.877025787862));
#25817=CARTESIAN_POINT('Ctrl Pts',(198.695346748023,95.7772376084047,338.076892623358));
#25818=CARTESIAN_POINT('Ctrl Pts',(199.108193617031,95.7147376084047,336.276759458854));
#25819=CARTESIAN_POINT('Ctrl Pts',(200.673006805358,95.6522376084047,335.295799911861));
#25820=CARTESIAN_POINT('Ctrl Pts',(202.237819993686,95.5897376084047,334.314840364869));
#25821=CARTESIAN_POINT('Ctrl Pts',(204.03795315819,95.5272376084047,334.727687233877));
#25822=CARTESIAN_POINT('Ctrl Pts',(205.838086322694,95.4647376084047,335.140534102886));
#25823=CARTESIAN_POINT('Ctrl Pts',(206.819045869686,95.4022376084047,336.705347291213));
#25824=CARTESIAN_POINT('Ctrl Pts',(207.800005416678,95.3397376084047,338.27016047954));
#25825=CARTESIAN_POINT('Ctrl Pts',(207.38715854767,95.2772376084047,340.070293644044));
#25826=CARTESIAN_POINT('Ctrl Pts',(206.974311678662,95.2147376084047,341.870426808548));
#25827=CARTESIAN_POINT('Ctrl Pts',(205.409498490334,95.1522376084047,342.851386355541));
#25828=CARTESIAN_POINT('Ctrl Pts',(203.844685302007,95.0897376084047,343.832345902533));
#25829=CARTESIAN_POINT('Ctrl Pts',(202.044552137503,95.0272376084047,343.419499033524));
#25830=CARTESIAN_POINT('Ctrl Pts',(200.244418972999,94.9647376084047,343.006652164516));
#25831=CARTESIAN_POINT('Ctrl Pts',(199.263459426007,94.9022376084047,341.441838976189));
#25832=CARTESIAN_POINT('Ctrl Pts',(198.282499879015,94.8397376084047,339.877025787862));
#25833=CARTESIAN_POINT('Ctrl Pts',(198.695346748023,94.7772376084047,338.076892623358));
#25834=CARTESIAN_POINT('Ctrl Pts',(199.108193617031,94.7147376084047,336.276759458854));
#25835=CARTESIAN_POINT('Ctrl Pts',(200.673006805358,94.6522376084047,335.295799911861));
#25836=CARTESIAN_POINT('Ctrl Pts',(202.237819993686,94.5897376084047,334.314840364869));
#25837=CARTESIAN_POINT('Ctrl Pts',(204.03795315819,94.5272376084047,334.727687233877));
#25838=CARTESIAN_POINT('Ctrl Pts',(205.838086322694,94.4647376084047,335.140534102886));
#25839=CARTESIAN_POINT('Ctrl Pts',(206.819045869686,94.4022376084047,336.705347291213));
#25840=CARTESIAN_POINT('Ctrl Pts',(207.800005416678,94.3397376084047,338.27016047954));
#25841=CARTESIAN_POINT('Ctrl Pts',(207.38715854767,94.2772376084047,340.070293644044));
#25842=CARTESIAN_POINT('Ctrl Pts',(206.974311678662,94.2147376084047,341.870426808548));
#25843=CARTESIAN_POINT('Ctrl Pts',(205.409498490334,94.1522376084047,342.851386355541));
#25844=CARTESIAN_POINT('Ctrl Pts',(203.844685302007,94.0897376084047,343.832345902533));
#25845=CARTESIAN_POINT('Ctrl Pts',(202.044552137503,94.0272376084047,343.419499033524));
#25846=CARTESIAN_POINT('Ctrl Pts',(200.244418972999,93.9647376084047,343.006652164516));
#25847=CARTESIAN_POINT('Ctrl Pts',(199.263459426007,93.9022376084047,341.441838976189));
#25848=CARTESIAN_POINT('Ctrl Pts',(198.282499879015,93.8397376084047,339.877025787862));
#25849=CARTESIAN_POINT('Ctrl Pts',(198.695346748023,93.7772376084047,338.076892623358));
#25850=CARTESIAN_POINT('Ctrl Pts',(199.108193617031,93.7147376084047,336.276759458854));
#25851=CARTESIAN_POINT('Ctrl Pts',(200.673006805358,93.6522376084047,335.295799911861));
#25852=CARTESIAN_POINT('Ctrl Pts',(202.237819993686,93.5897376084047,334.314840364869));
#25853=CARTESIAN_POINT('Ctrl Pts',(204.03795315819,93.5272376084047,334.727687233877));
#25854=CARTESIAN_POINT('Ctrl Pts',(205.838086322694,93.4647376084047,335.140534102886));
#25855=CARTESIAN_POINT('Ctrl Pts',(206.819045869686,93.4022376084047,336.705347291213));
#25856=CARTESIAN_POINT('Ctrl Pts',(207.800005416678,93.3397376084047,338.27016047954));
#25857=CARTESIAN_POINT('Ctrl Pts',(207.38715854767,93.2772376084047,340.070293644044));
#25858=CARTESIAN_POINT('Ctrl Pts',(206.974311678662,93.2147376084047,341.870426808548));
#25859=CARTESIAN_POINT('Ctrl Pts',(205.409498490334,93.1522376084047,342.851386355541));
#25860=CARTESIAN_POINT('Ctrl Pts',(203.844685302007,93.0897376084047,343.832345902533));
#25861=CARTESIAN_POINT('Ctrl Pts',(202.044552137503,93.0272376084047,343.419499033524));
#25862=CARTESIAN_POINT('Ctrl Pts',(200.244418972999,92.9647376084047,343.006652164516));
#25863=CARTESIAN_POINT('Ctrl Pts',(199.263459426007,92.9022376084047,341.441838976189));
#25864=CARTESIAN_POINT('Ctrl Pts',(198.282499879015,92.8397376084047,339.877025787862));
#25865=CARTESIAN_POINT('Ctrl Pts',(198.695346748023,92.7772376084047,338.076892623358));
#25866=CARTESIAN_POINT('Ctrl Pts',(199.108193617031,92.7147376084047,336.276759458854));
#25867=CARTESIAN_POINT('Ctrl Pts',(200.673006805358,92.6522376084047,335.295799911861));
#25868=CARTESIAN_POINT('Ctrl Pts',(202.237819993686,92.5897376084047,334.314840364869));
#25869=CARTESIAN_POINT('Ctrl Pts',(204.03795315819,92.5272376084047,334.727687233877));
#25870=CARTESIAN_POINT('Ctrl Pts',(205.838086322694,92.4647376084047,335.140534102886));
#25871=CARTESIAN_POINT('Ctrl Pts',(206.819045869686,92.4022376084047,336.705347291213));
#25872=CARTESIAN_POINT('Ctrl Pts',(207.800005416678,92.3397376084047,338.27016047954));
#25873=CARTESIAN_POINT('Ctrl Pts',(207.38715854767,92.2772376084047,340.070293644044));
#25874=CARTESIAN_POINT('Ctrl Pts',(206.974311678662,92.2147376084047,341.870426808548));
#25875=CARTESIAN_POINT('Ctrl Pts',(205.409498490334,92.1522376084047,342.851386355541));
#25876=CARTESIAN_POINT('Ctrl Pts',(203.844685302007,92.0897376084047,343.832345902533));
#25877=CARTESIAN_POINT('Ctrl Pts',(202.044552137503,92.0272376084047,343.419499033524));
#25878=CARTESIAN_POINT('Ctrl Pts',(200.244418972999,91.9647376084047,343.006652164516));
#25879=CARTESIAN_POINT('Ctrl Pts',(199.263459426007,91.9022376084047,341.441838976189));
#25880=CARTESIAN_POINT('Ctrl Pts',(198.282499879015,91.8397376084047,339.877025787862));
#25881=CARTESIAN_POINT('Ctrl Pts',(198.695346748023,91.7772376084047,338.076892623358));
#25882=CARTESIAN_POINT('Ctrl Pts',(199.108193617031,91.7147376084047,336.276759458854));
#25883=CARTESIAN_POINT('Ctrl Pts',(200.673006805358,91.6522376084047,335.295799911861));
#25884=CARTESIAN_POINT('Ctrl Pts',(202.237819993686,91.5897376084047,334.314840364869));
#25885=CARTESIAN_POINT('Ctrl Pts',(204.03795315819,91.5272376084047,334.727687233877));
#25886=CARTESIAN_POINT('Ctrl Pts',(205.838086322694,91.4647376084047,335.140534102886));
#25887=CARTESIAN_POINT('Ctrl Pts',(206.819045869686,91.4022376084047,336.705347291213));
#25888=CARTESIAN_POINT('Ctrl Pts',(207.800005416678,91.3397376084047,338.27016047954));
#25889=CARTESIAN_POINT('Ctrl Pts',(207.38715854767,91.2772376084047,340.070293644044));
#25890=CARTESIAN_POINT('Ctrl Pts',(206.974311678662,91.2147376084047,341.870426808548));
#25891=CARTESIAN_POINT('Ctrl Pts',(205.409498490334,91.1522376084047,342.851386355541));
#25892=CARTESIAN_POINT('Ctrl Pts',(203.844685302007,91.0897376084047,343.832345902533));
#25893=CARTESIAN_POINT('Ctrl Pts',(202.044552137503,91.0272376084047,343.419499033524));
#25894=CARTESIAN_POINT('Ctrl Pts',(200.244418972999,90.9647376084047,343.006652164516));
#25895=CARTESIAN_POINT('Ctrl Pts',(199.263459426007,90.9022376084047,341.441838976189));
#25896=CARTESIAN_POINT('Ctrl Pts',(198.282499879015,90.8397376084047,339.877025787862));
#25897=CARTESIAN_POINT('Ctrl Pts',(198.695346748023,90.7772376084047,338.076892623358));
#25898=CARTESIAN_POINT('Ctrl Pts',(199.108193617031,90.7147376084047,336.276759458854));
#25899=CARTESIAN_POINT('Ctrl Pts',(200.673006805358,90.6522376084047,335.295799911861));
#25900=CARTESIAN_POINT('Ctrl Pts',(202.237819993686,90.5897376084047,334.314840364869));
#25901=CARTESIAN_POINT('Ctrl Pts',(204.03795315819,90.5272376084047,334.727687233877));
#25902=CARTESIAN_POINT('Ctrl Pts',(205.838086322694,90.4647376084047,335.140534102886));
#25903=CARTESIAN_POINT('Ctrl Pts',(206.819045869686,90.4022376084047,336.705347291213));
#25904=CARTESIAN_POINT('Ctrl Pts',(207.800005416678,90.3397376084047,338.27016047954));
#25905=CARTESIAN_POINT('Ctrl Pts',(207.38715854767,90.2772376084047,340.070293644044));
#25906=CARTESIAN_POINT('Ctrl Pts',(206.974311678662,90.2147376084047,341.870426808548));
#25907=CARTESIAN_POINT('Ctrl Pts',(205.409498490334,90.1522376084047,342.851386355541));
#25908=CARTESIAN_POINT('Ctrl Pts',(203.844685302007,90.0897376084047,343.832345902533));
#25909=CARTESIAN_POINT('Ctrl Pts',(202.044552137503,90.0272376084047,343.419499033524));
#25910=CARTESIAN_POINT('Ctrl Pts',(200.244418972999,89.9647376084047,343.006652164516));
#25911=CARTESIAN_POINT('Ctrl Pts',(199.263459426007,89.9022376084047,341.441838976189));
#25912=CARTESIAN_POINT('Ctrl Pts',(198.282499879015,89.8397376084047,339.877025787862));
#25913=CARTESIAN_POINT('Ctrl Pts',(198.695346748023,89.7772376084047,338.076892623358));
#25914=CARTESIAN_POINT('Ctrl Pts',(199.108193617031,89.7147376084047,336.276759458854));
#25915=CARTESIAN_POINT('Ctrl Pts',(200.673006805358,89.6522376084047,335.295799911861));
#25916=CARTESIAN_POINT('Ctrl Pts',(202.237819993686,89.5897376084047,334.314840364869));
#25917=CARTESIAN_POINT('Ctrl Pts',(204.03795315819,89.5272376084047,334.727687233877));
#25918=CARTESIAN_POINT('Ctrl Pts',(205.838086322694,89.4647376084047,335.140534102886));
#25919=CARTESIAN_POINT('Ctrl Pts',(206.819045869686,89.4022376084047,336.705347291213));
#25920=CARTESIAN_POINT('Ctrl Pts',(207.800005416678,89.3397376084047,338.27016047954));
#25921=CARTESIAN_POINT('Ctrl Pts',(207.38715854767,89.2772376084047,340.070293644044));
#25922=CARTESIAN_POINT('Ctrl Pts',(206.974311678662,89.2147376084047,341.870426808548));
#25923=CARTESIAN_POINT('Ctrl Pts',(205.409498490334,89.1522376084047,342.851386355541));
#25924=CARTESIAN_POINT('Ctrl Pts',(203.844685302007,89.0897376084047,343.832345902533));
#25925=CARTESIAN_POINT('Ctrl Pts',(202.044552137503,89.0272376084047,343.419499033524));
#25926=CARTESIAN_POINT('Ctrl Pts',(200.244418972999,88.9647376084047,343.006652164516));
#25927=CARTESIAN_POINT('Ctrl Pts',(199.263459426007,88.9022376084047,341.441838976189));
#25928=CARTESIAN_POINT('Ctrl Pts',(198.282499879015,88.8397376084047,339.877025787862));
#25929=CARTESIAN_POINT('Ctrl Pts',(198.695346748023,88.7772376084047,338.076892623358));
#25930=CARTESIAN_POINT('Ctrl Pts',(199.108193617031,88.7147376084047,336.276759458854));
#25931=CARTESIAN_POINT('Ctrl Pts',(200.673006805358,88.6522376084047,335.295799911861));
#25932=CARTESIAN_POINT('Ctrl Pts',(202.237819993686,88.5897376084047,334.314840364869));
#25933=CARTESIAN_POINT('Ctrl Pts',(204.03795315819,88.5272376084047,334.727687233877));
#25934=CARTESIAN_POINT('Ctrl Pts',(205.838086322694,88.4647376084047,335.140534102886));
#25935=CARTESIAN_POINT('Ctrl Pts',(206.819045869686,88.4022376084047,336.705347291213));
#25936=CARTESIAN_POINT('Ctrl Pts',(207.800005416678,88.3397376084047,338.27016047954));
#25937=CARTESIAN_POINT('Ctrl Pts',(207.38715854767,88.2772376084047,340.070293644044));
#25938=CARTESIAN_POINT('Ctrl Pts',(206.974311678662,88.2147376084047,341.870426808548));
#25939=CARTESIAN_POINT('Ctrl Pts',(205.409498490334,88.1522376084047,342.851386355541));
#25940=CARTESIAN_POINT('Ctrl Pts',(203.844685302007,88.0897376084047,343.832345902533));
#25941=CARTESIAN_POINT('Ctrl Pts',(202.044552137503,88.0272376084047,343.419499033524));
#25942=CARTESIAN_POINT('Ctrl Pts',(200.244418972999,87.9647376084047,343.006652164516));
#25943=CARTESIAN_POINT('Ctrl Pts',(199.263459426007,87.9022376084047,341.441838976189));
#25944=CARTESIAN_POINT('Ctrl Pts',(198.282499879015,87.8397376084047,339.877025787862));
#25945=CARTESIAN_POINT('Ctrl Pts',(198.695346748023,87.7772376084047,338.076892623358));
#25946=CARTESIAN_POINT('Ctrl Pts',(199.108193617031,87.7147376084047,336.276759458854));
#25947=CARTESIAN_POINT('Ctrl Pts',(200.673006805358,87.6522376084047,335.295799911861));
#25948=CARTESIAN_POINT('Ctrl Pts',(202.237819993686,87.5897376084047,334.314840364869));
#25949=CARTESIAN_POINT('Ctrl Pts',(204.03795315819,87.5272376084047,334.727687233877));
#25950=CARTESIAN_POINT('Origin',(224.770541810138,65.2397376070391,333.797420988906));
#25951=CARTESIAN_POINT('Origin',(220.299763861057,65.2397376070391,353.291321176658));
#25952=CARTESIAN_POINT('Origin',(220.299763861057,65.2397376070391,353.291321176658));
#25953=CARTESIAN_POINT('Origin',(224.770541810138,65.2397376070391,333.797420988906));
#25954=CARTESIAN_POINT('Origin',(203.041252647848,99.3647376084047,339.073593133703));
#25955=CARTESIAN_POINT('',(208.562910255543,96.8022376084046,339.539344956919));
#25956=CARTESIAN_POINT('',(208.562910255543,96.9272376084047,339.539344956919));
#25957=CARTESIAN_POINT('',(208.562910255543,99.3647376084047,339.539344956919));
#25958=CARTESIAN_POINT('',(204.724000912662,97.739737607039,344.353175103396));
#25959=CARTESIAN_POINT('Ctrl Pts',(204.724000912662,97.739737607039,344.353175103396));
#25960=CARTESIAN_POINT('Ctrl Pts',(203.673826787241,97.7072511661896,344.687894537141));
#25961=CARTESIAN_POINT('Ctrl Pts',(202.575500824633,97.6772376084047,344.595250741398));
#25962=CARTESIAN_POINT('Ctrl Pts',(200.288355356745,97.6147376084047,344.402330019522));
#25963=CARTESIAN_POINT('Ctrl Pts',(198.807514837511,97.5522376084047,342.648658398949));
#25964=CARTESIAN_POINT('Ctrl Pts',(197.326674318278,97.4897376084047,340.894986778376));
#25965=CARTESIAN_POINT('Ctrl Pts',(197.519595040153,97.4272376084047,338.607841310488));
#25966=CARTESIAN_POINT('Ctrl Pts',(197.712515762029,97.3647376084047,336.320695842601));
#25967=CARTESIAN_POINT('Ctrl Pts',(199.466187382602,97.3022376084047,334.839855323367));
#25968=CARTESIAN_POINT('Ctrl Pts',(201.219859003176,97.2397376084047,333.359014804133));
#25969=CARTESIAN_POINT('Ctrl Pts',(203.507004471063,97.1772376084047,333.551935526009));
#25970=CARTESIAN_POINT('Ctrl Pts',(205.794149938951,97.1147376084047,333.744856247885));
#25971=CARTESIAN_POINT('Ctrl Pts',(207.274990458185,97.0522376084047,335.498527868458));
#25972=CARTESIAN_POINT('Ctrl Pts',(208.755830977418,96.9897376084047,337.252199489031));
#25973=CARTESIAN_POINT('Ctrl Pts',(208.562910255543,96.9272376084047,339.539344956919));
#25974=CARTESIAN_POINT('',(207.964363569528,97.739737607039,341.616938637223));
#25975=CARTESIAN_POINT('Origin',(203.041252647847,97.7397376070395,339.073593133703));
#25976=CARTESIAN_POINT('Ctrl Pts',(207.964363569528,97.7397376070391,341.616938637223));
#25977=CARTESIAN_POINT('Ctrl Pts',(207.458460705412,97.7072511661896,342.596206264131));
#25978=CARTESIAN_POINT('Ctrl Pts',(206.616317913094,97.6772376084047,343.30733094404));
#25979=CARTESIAN_POINT('Ctrl Pts',(204.86264629252,97.6147376084047,344.788171463274));
#25980=CARTESIAN_POINT('Ctrl Pts',(202.575500824633,97.5522376084047,344.595250741398));
#25981=CARTESIAN_POINT('Ctrl Pts',(200.288355356745,97.4897376084047,344.402330019522));
#25982=CARTESIAN_POINT('Ctrl Pts',(198.807514837511,97.4272376084047,342.648658398949));
#25983=CARTESIAN_POINT('Ctrl Pts',(197.326674318278,97.3647376084047,340.894986778376));
#25984=CARTESIAN_POINT('Ctrl Pts',(197.519595040153,97.3022376084047,338.607841310488));
#25985=CARTESIAN_POINT('Ctrl Pts',(197.712515762029,97.2397376084047,336.320695842601));
#25986=CARTESIAN_POINT('Ctrl Pts',(199.466187382602,97.1772376084047,334.839855323367));
#25987=CARTESIAN_POINT('Ctrl Pts',(201.219859003176,97.1147376084047,333.359014804133));
#25988=CARTESIAN_POINT('Ctrl Pts',(203.507004471063,97.0522376084047,333.551935526009));
#25989=CARTESIAN_POINT('Ctrl Pts',(205.794149938951,96.9897376084047,333.744856247885));
#25990=CARTESIAN_POINT('Ctrl Pts',(207.274990458185,96.9272376084047,335.498527868458));
#25991=CARTESIAN_POINT('Ctrl Pts',(208.755830977418,96.8647376084047,337.252199489031));
#25992=CARTESIAN_POINT('Ctrl Pts',(208.562910255543,96.8022376084046,339.539344956919));
#25993=CARTESIAN_POINT('Origin',(203.041252647848,99.3647376084047,339.073593133703));
#25994=CARTESIAN_POINT('',(208.562910255543,95.8022376084047,339.539344956919));
#25995=CARTESIAN_POINT('',(208.562910255543,95.9272376084047,339.539344956919));
#25996=CARTESIAN_POINT('',(208.562910255543,99.3647376084047,339.539344956919));
#25997=CARTESIAN_POINT('Ctrl Pts',(208.562910255543,96.9272376084047,339.539344956919));
#25998=CARTESIAN_POINT('Ctrl Pts',(208.369989533667,96.8647376084047,341.826490424806));
#25999=CARTESIAN_POINT('Ctrl Pts',(206.616317913094,96.8022376084046,343.30733094404));
#26000=CARTESIAN_POINT('Ctrl Pts',(204.86264629252,96.7397376084047,344.788171463274));
#26001=CARTESIAN_POINT('Ctrl Pts',(202.575500824633,96.6772376084047,344.595250741398));
#26002=CARTESIAN_POINT('Ctrl Pts',(200.288355356745,96.6147376084047,344.402330019522));
#26003=CARTESIAN_POINT('Ctrl Pts',(198.807514837511,96.5522376084046,342.648658398949));
#26004=CARTESIAN_POINT('Ctrl Pts',(197.326674318278,96.4897376084047,340.894986778376));
#26005=CARTESIAN_POINT('Ctrl Pts',(197.519595040153,96.4272376084047,338.607841310488));
#26006=CARTESIAN_POINT('Ctrl Pts',(197.712515762029,96.3647376084047,336.320695842601));
#26007=CARTESIAN_POINT('Ctrl Pts',(199.466187382602,96.3022376084047,334.839855323367));
#26008=CARTESIAN_POINT('Ctrl Pts',(201.219859003176,96.2397376084047,333.359014804133));
#26009=CARTESIAN_POINT('Ctrl Pts',(203.507004471063,96.1772376084047,333.551935526009));
#26010=CARTESIAN_POINT('Ctrl Pts',(205.794149938951,96.1147376084047,333.744856247885));
#26011=CARTESIAN_POINT('Ctrl Pts',(207.274990458185,96.0522376084047,335.498527868458));
#26012=CARTESIAN_POINT('Ctrl Pts',(208.755830977418,95.9897376084047,337.252199489031));
#26013=CARTESIAN_POINT('Ctrl Pts',(208.562910255543,95.9272376084047,339.539344956919));
#26014=CARTESIAN_POINT('Ctrl Pts',(208.562910255543,96.8022376084046,339.539344956919));
#26015=CARTESIAN_POINT('Ctrl Pts',(208.369989533667,96.7397376084047,341.826490424806));
#26016=CARTESIAN_POINT('Ctrl Pts',(206.616317913094,96.6772376084047,343.30733094404));
#26017=CARTESIAN_POINT('Ctrl Pts',(204.86264629252,96.6147376084047,344.788171463274));
#26018=CARTESIAN_POINT('Ctrl Pts',(202.575500824633,96.5522376084046,344.595250741398));
#26019=CARTESIAN_POINT('Ctrl Pts',(200.288355356745,96.4897376084047,344.402330019522));
#26020=CARTESIAN_POINT('Ctrl Pts',(198.807514837511,96.4272376084047,342.648658398949));
#26021=CARTESIAN_POINT('Ctrl Pts',(197.326674318278,96.3647376084047,340.894986778376));
#26022=CARTESIAN_POINT('Ctrl Pts',(197.519595040153,96.3022376084047,338.607841310488));
#26023=CARTESIAN_POINT('Ctrl Pts',(197.712515762029,96.2397376084047,336.320695842601));
#26024=CARTESIAN_POINT('Ctrl Pts',(199.466187382602,96.1772376084047,334.839855323367));
#26025=CARTESIAN_POINT('Ctrl Pts',(201.219859003176,96.1147376084047,333.359014804133));
#26026=CARTESIAN_POINT('Ctrl Pts',(203.507004471063,96.0522376084047,333.551935526009));
#26027=CARTESIAN_POINT('Ctrl Pts',(205.794149938951,95.9897376084047,333.744856247885));
#26028=CARTESIAN_POINT('Ctrl Pts',(207.274990458185,95.9272376084047,335.498527868458));
#26029=CARTESIAN_POINT('Ctrl Pts',(208.755830977418,95.8647376084047,337.252199489031));
#26030=CARTESIAN_POINT('Ctrl Pts',(208.562910255543,95.8022376084047,339.539344956919));
#26031=CARTESIAN_POINT('Origin',(203.041252647848,99.3647376084047,339.073593133703));
#26032=CARTESIAN_POINT('',(208.562910255543,94.8022376084047,339.539344956919));
#26033=CARTESIAN_POINT('',(208.562910255543,94.9272376084047,339.539344956919));
#26034=CARTESIAN_POINT('',(208.562910255543,99.3647376084047,339.539344956919));
#26035=CARTESIAN_POINT('Ctrl Pts',(208.562910255543,95.9272376084047,339.539344956919));
#26036=CARTESIAN_POINT('Ctrl Pts',(208.369989533667,95.8647376084047,341.826490424806));
#26037=CARTESIAN_POINT('Ctrl Pts',(206.616317913094,95.8022376084047,343.30733094404));
#26038=CARTESIAN_POINT('Ctrl Pts',(204.86264629252,95.7397376084047,344.788171463274));
#26039=CARTESIAN_POINT('Ctrl Pts',(202.575500824633,95.6772376084046,344.595250741398));
#26040=CARTESIAN_POINT('Ctrl Pts',(200.288355356745,95.6147376084047,344.402330019522));
#26041=CARTESIAN_POINT('Ctrl Pts',(198.807514837511,95.5522376084046,342.648658398949));
#26042=CARTESIAN_POINT('Ctrl Pts',(197.326674318278,95.4897376084047,340.894986778376));
#26043=CARTESIAN_POINT('Ctrl Pts',(197.519595040153,95.4272376084047,338.607841310488));
#26044=CARTESIAN_POINT('Ctrl Pts',(197.712515762029,95.3647376084047,336.320695842601));
#26045=CARTESIAN_POINT('Ctrl Pts',(199.466187382602,95.3022376084047,334.839855323367));
#26046=CARTESIAN_POINT('Ctrl Pts',(201.219859003176,95.2397376084047,333.359014804133));
#26047=CARTESIAN_POINT('Ctrl Pts',(203.507004471063,95.1772376084047,333.551935526009));
#26048=CARTESIAN_POINT('Ctrl Pts',(205.794149938951,95.1147376084047,333.744856247885));
#26049=CARTESIAN_POINT('Ctrl Pts',(207.274990458185,95.0522376084046,335.498527868458));
#26050=CARTESIAN_POINT('Ctrl Pts',(208.755830977418,94.9897376084047,337.252199489031));
#26051=CARTESIAN_POINT('Ctrl Pts',(208.562910255543,94.9272376084047,339.539344956919));
#26052=CARTESIAN_POINT('Ctrl Pts',(208.562910255543,95.8022376084047,339.539344956919));
#26053=CARTESIAN_POINT('Ctrl Pts',(208.369989533667,95.7397376084047,341.826490424806));
#26054=CARTESIAN_POINT('Ctrl Pts',(206.616317913094,95.6772376084046,343.30733094404));
#26055=CARTESIAN_POINT('Ctrl Pts',(204.86264629252,95.6147376084047,344.788171463274));
#26056=CARTESIAN_POINT('Ctrl Pts',(202.575500824633,95.5522376084046,344.595250741398));
#26057=CARTESIAN_POINT('Ctrl Pts',(200.288355356745,95.4897376084047,344.402330019522));
#26058=CARTESIAN_POINT('Ctrl Pts',(198.807514837511,95.4272376084047,342.648658398949));
#26059=CARTESIAN_POINT('Ctrl Pts',(197.326674318278,95.3647376084047,340.894986778376));
#26060=CARTESIAN_POINT('Ctrl Pts',(197.519595040153,95.3022376084046,338.607841310488));
#26061=CARTESIAN_POINT('Ctrl Pts',(197.712515762029,95.2397376084047,336.320695842601));
#26062=CARTESIAN_POINT('Ctrl Pts',(199.466187382602,95.1772376084047,334.839855323367));
#26063=CARTESIAN_POINT('Ctrl Pts',(201.219859003176,95.1147376084047,333.359014804133));
#26064=CARTESIAN_POINT('Ctrl Pts',(203.507004471063,95.0522376084047,333.551935526009));
#26065=CARTESIAN_POINT('Ctrl Pts',(205.794149938951,94.9897376084047,333.744856247885));
#26066=CARTESIAN_POINT('Ctrl Pts',(207.274990458185,94.9272376084047,335.498527868458));
#26067=CARTESIAN_POINT('Ctrl Pts',(208.755830977418,94.8647376084047,337.252199489031));
#26068=CARTESIAN_POINT('Ctrl Pts',(208.562910255543,94.8022376084047,339.539344956919));
#26069=CARTESIAN_POINT('Origin',(203.041252647848,99.3647376084047,339.073593133703));
#26070=CARTESIAN_POINT('',(208.562910255543,93.8022376084047,339.539344956919));
#26071=CARTESIAN_POINT('',(208.562910255543,93.9272376084047,339.539344956919));
#26072=CARTESIAN_POINT('',(208.562910255543,99.3647376084047,339.539344956919));
#26073=CARTESIAN_POINT('Ctrl Pts',(208.562910255543,94.9272376084047,339.539344956919));
#26074=CARTESIAN_POINT('Ctrl Pts',(208.369989533667,94.8647376084047,341.826490424806));
#26075=CARTESIAN_POINT('Ctrl Pts',(206.616317913094,94.8022376084047,343.30733094404));
#26076=CARTESIAN_POINT('Ctrl Pts',(204.86264629252,94.7397376084047,344.788171463274));
#26077=CARTESIAN_POINT('Ctrl Pts',(202.575500824633,94.6772376084047,344.595250741398));
#26078=CARTESIAN_POINT('Ctrl Pts',(200.288355356745,94.6147376084047,344.402330019522));
#26079=CARTESIAN_POINT('Ctrl Pts',(198.807514837511,94.5522376084047,342.648658398949));
#26080=CARTESIAN_POINT('Ctrl Pts',(197.326674318278,94.4897376084047,340.894986778376));
#26081=CARTESIAN_POINT('Ctrl Pts',(197.519595040153,94.4272376084047,338.607841310488));
#26082=CARTESIAN_POINT('Ctrl Pts',(197.712515762029,94.3647376084047,336.320695842601));
#26083=CARTESIAN_POINT('Ctrl Pts',(199.466187382602,94.3022376084047,334.839855323367));
#26084=CARTESIAN_POINT('Ctrl Pts',(201.219859003176,94.2397376084047,333.359014804133));
#26085=CARTESIAN_POINT('Ctrl Pts',(203.507004471063,94.1772376084047,333.551935526009));
#26086=CARTESIAN_POINT('Ctrl Pts',(205.794149938951,94.1147376084047,333.744856247885));
#26087=CARTESIAN_POINT('Ctrl Pts',(207.274990458185,94.0522376084047,335.498527868458));
#26088=CARTESIAN_POINT('Ctrl Pts',(208.755830977418,93.9897376084047,337.252199489031));
#26089=CARTESIAN_POINT('Ctrl Pts',(208.562910255543,93.9272376084047,339.539344956919));
#26090=CARTESIAN_POINT('Ctrl Pts',(208.562910255543,94.8022376084047,339.539344956919));
#26091=CARTESIAN_POINT('Ctrl Pts',(208.369989533667,94.7397376084047,341.826490424806));
#26092=CARTESIAN_POINT('Ctrl Pts',(206.616317913094,94.6772376084047,343.30733094404));
#26093=CARTESIAN_POINT('Ctrl Pts',(204.86264629252,94.6147376084047,344.788171463274));
#26094=CARTESIAN_POINT('Ctrl Pts',(202.575500824633,94.5522376084047,344.595250741398));
#26095=CARTESIAN_POINT('Ctrl Pts',(200.288355356745,94.4897376084047,344.402330019522));
#26096=CARTESIAN_POINT('Ctrl Pts',(198.807514837511,94.4272376084047,342.648658398949));
#26097=CARTESIAN_POINT('Ctrl Pts',(197.326674318278,94.3647376084047,340.894986778376));
#26098=CARTESIAN_POINT('Ctrl Pts',(197.519595040153,94.3022376084047,338.607841310488));
#26099=CARTESIAN_POINT('Ctrl Pts',(197.712515762029,94.2397376084047,336.320695842601));
#26100=CARTESIAN_POINT('Ctrl Pts',(199.466187382602,94.1772376084047,334.839855323367));
#26101=CARTESIAN_POINT('Ctrl Pts',(201.219859003176,94.1147376084047,333.359014804133));
#26102=CARTESIAN_POINT('Ctrl Pts',(203.507004471063,94.0522376084047,333.551935526009));
#26103=CARTESIAN_POINT('Ctrl Pts',(205.794149938951,93.9897376084047,333.744856247885));
#26104=CARTESIAN_POINT('Ctrl Pts',(207.274990458185,93.9272376084047,335.498527868458));
#26105=CARTESIAN_POINT('Ctrl Pts',(208.755830977418,93.8647376084047,337.252199489031));
#26106=CARTESIAN_POINT('Ctrl Pts',(208.562910255543,93.8022376084047,339.539344956919));
#26107=CARTESIAN_POINT('Origin',(203.041252647848,99.3647376084047,339.073593133703));
#26108=CARTESIAN_POINT('',(208.562910255543,92.8022376084047,339.539344956919));
#26109=CARTESIAN_POINT('',(208.562910255543,92.9272376084047,339.539344956919));
#26110=CARTESIAN_POINT('',(208.562910255543,99.3647376084047,339.539344956919));
#26111=CARTESIAN_POINT('Ctrl Pts',(208.562910255543,93.9272376084047,339.539344956919));
#26112=CARTESIAN_POINT('Ctrl Pts',(208.369989533667,93.8647376084047,341.826490424806));
#26113=CARTESIAN_POINT('Ctrl Pts',(206.616317913094,93.8022376084047,343.30733094404));
#26114=CARTESIAN_POINT('Ctrl Pts',(204.86264629252,93.7397376084047,344.788171463274));
#26115=CARTESIAN_POINT('Ctrl Pts',(202.575500824633,93.6772376084047,344.595250741398));
#26116=CARTESIAN_POINT('Ctrl Pts',(200.288355356745,93.6147376084047,344.402330019522));
#26117=CARTESIAN_POINT('Ctrl Pts',(198.807514837511,93.5522376084047,342.648658398949));
#26118=CARTESIAN_POINT('Ctrl Pts',(197.326674318278,93.4897376084047,340.894986778376));
#26119=CARTESIAN_POINT('Ctrl Pts',(197.519595040153,93.4272376084047,338.607841310488));
#26120=CARTESIAN_POINT('Ctrl Pts',(197.712515762029,93.3647376084047,336.320695842601));
#26121=CARTESIAN_POINT('Ctrl Pts',(199.466187382602,93.3022376084047,334.839855323367));
#26122=CARTESIAN_POINT('Ctrl Pts',(201.219859003176,93.2397376084047,333.359014804133));
#26123=CARTESIAN_POINT('Ctrl Pts',(203.507004471063,93.1772376084047,333.551935526009));
#26124=CARTESIAN_POINT('Ctrl Pts',(205.794149938951,93.1147376084047,333.744856247885));
#26125=CARTESIAN_POINT('Ctrl Pts',(207.274990458185,93.0522376084047,335.498527868458));
#26126=CARTESIAN_POINT('Ctrl Pts',(208.755830977418,92.9897376084047,337.252199489031));
#26127=CARTESIAN_POINT('Ctrl Pts',(208.562910255543,92.9272376084047,339.539344956919));
#26128=CARTESIAN_POINT('Ctrl Pts',(208.562910255543,93.8022376084047,339.539344956919));
#26129=CARTESIAN_POINT('Ctrl Pts',(208.369989533667,93.7397376084047,341.826490424806));
#26130=CARTESIAN_POINT('Ctrl Pts',(206.616317913094,93.6772376084047,343.30733094404));
#26131=CARTESIAN_POINT('Ctrl Pts',(204.86264629252,93.6147376084047,344.788171463274));
#26132=CARTESIAN_POINT('Ctrl Pts',(202.575500824633,93.5522376084047,344.595250741398));
#26133=CARTESIAN_POINT('Ctrl Pts',(200.288355356745,93.4897376084047,344.402330019522));
#26134=CARTESIAN_POINT('Ctrl Pts',(198.807514837511,93.4272376084047,342.648658398949));
#26135=CARTESIAN_POINT('Ctrl Pts',(197.326674318278,93.3647376084047,340.894986778376));
#26136=CARTESIAN_POINT('Ctrl Pts',(197.519595040153,93.3022376084047,338.607841310488));
#26137=CARTESIAN_POINT('Ctrl Pts',(197.712515762029,93.2397376084047,336.320695842601));
#26138=CARTESIAN_POINT('Ctrl Pts',(199.466187382602,93.1772376084047,334.839855323367));
#26139=CARTESIAN_POINT('Ctrl Pts',(201.219859003176,93.1147376084047,333.359014804133));
#26140=CARTESIAN_POINT('Ctrl Pts',(203.507004471063,93.0522376084047,333.551935526009));
#26141=CARTESIAN_POINT('Ctrl Pts',(205.794149938951,92.9897376084047,333.744856247885));
#26142=CARTESIAN_POINT('Ctrl Pts',(207.274990458185,92.9272376084047,335.498527868458));
#26143=CARTESIAN_POINT('Ctrl Pts',(208.755830977418,92.8647376084047,337.252199489031));
#26144=CARTESIAN_POINT('Ctrl Pts',(208.562910255543,92.8022376084047,339.539344956919));
#26145=CARTESIAN_POINT('Origin',(203.041252647848,99.3647376084047,339.073593133703));
#26146=CARTESIAN_POINT('',(208.562910255543,91.8022376084047,339.539344956919));
#26147=CARTESIAN_POINT('',(208.562910255543,91.9272376084047,339.539344956919));
#26148=CARTESIAN_POINT('',(208.562910255543,99.3647376084047,339.539344956919));
#26149=CARTESIAN_POINT('Ctrl Pts',(208.562910255543,92.9272376084047,339.539344956919));
#26150=CARTESIAN_POINT('Ctrl Pts',(208.369989533667,92.8647376084047,341.826490424806));
#26151=CARTESIAN_POINT('Ctrl Pts',(206.616317913094,92.8022376084047,343.30733094404));
#26152=CARTESIAN_POINT('Ctrl Pts',(204.86264629252,92.7397376084047,344.788171463274));
#26153=CARTESIAN_POINT('Ctrl Pts',(202.575500824633,92.6772376084047,344.595250741398));
#26154=CARTESIAN_POINT('Ctrl Pts',(200.288355356745,92.6147376084047,344.402330019522));
#26155=CARTESIAN_POINT('Ctrl Pts',(198.807514837511,92.5522376084047,342.648658398949));
#26156=CARTESIAN_POINT('Ctrl Pts',(197.326674318278,92.4897376084047,340.894986778376));
#26157=CARTESIAN_POINT('Ctrl Pts',(197.519595040153,92.4272376084047,338.607841310488));
#26158=CARTESIAN_POINT('Ctrl Pts',(197.712515762029,92.3647376084047,336.320695842601));
#26159=CARTESIAN_POINT('Ctrl Pts',(199.466187382602,92.3022376084047,334.839855323367));
#26160=CARTESIAN_POINT('Ctrl Pts',(201.219859003176,92.2397376084047,333.359014804133));
#26161=CARTESIAN_POINT('Ctrl Pts',(203.507004471063,92.1772376084047,333.551935526009));
#26162=CARTESIAN_POINT('Ctrl Pts',(205.794149938951,92.1147376084047,333.744856247885));
#26163=CARTESIAN_POINT('Ctrl Pts',(207.274990458185,92.0522376084047,335.498527868458));
#26164=CARTESIAN_POINT('Ctrl Pts',(208.755830977418,91.9897376084047,337.252199489031));
#26165=CARTESIAN_POINT('Ctrl Pts',(208.562910255543,91.9272376084047,339.539344956919));
#26166=CARTESIAN_POINT('Ctrl Pts',(208.562910255543,92.8022376084047,339.539344956919));
#26167=CARTESIAN_POINT('Ctrl Pts',(208.369989533667,92.7397376084047,341.826490424806));
#26168=CARTESIAN_POINT('Ctrl Pts',(206.616317913094,92.6772376084047,343.30733094404));
#26169=CARTESIAN_POINT('Ctrl Pts',(204.86264629252,92.6147376084047,344.788171463274));
#26170=CARTESIAN_POINT('Ctrl Pts',(202.575500824633,92.5522376084047,344.595250741398));
#26171=CARTESIAN_POINT('Ctrl Pts',(200.288355356745,92.4897376084047,344.402330019522));
#26172=CARTESIAN_POINT('Ctrl Pts',(198.807514837511,92.4272376084047,342.648658398949));
#26173=CARTESIAN_POINT('Ctrl Pts',(197.326674318278,92.3647376084047,340.894986778376));
#26174=CARTESIAN_POINT('Ctrl Pts',(197.519595040153,92.3022376084047,338.607841310488));
#26175=CARTESIAN_POINT('Ctrl Pts',(197.712515762029,92.2397376084047,336.320695842601));
#26176=CARTESIAN_POINT('Ctrl Pts',(199.466187382602,92.1772376084047,334.839855323367));
#26177=CARTESIAN_POINT('Ctrl Pts',(201.219859003176,92.1147376084047,333.359014804133));
#26178=CARTESIAN_POINT('Ctrl Pts',(203.507004471063,92.0522376084047,333.551935526009));
#26179=CARTESIAN_POINT('Ctrl Pts',(205.794149938951,91.9897376084047,333.744856247885));
#26180=CARTESIAN_POINT('Ctrl Pts',(207.274990458185,91.9272376084047,335.498527868458));
#26181=CARTESIAN_POINT('Ctrl Pts',(208.755830977418,91.8647376084047,337.252199489031));
#26182=CARTESIAN_POINT('Ctrl Pts',(208.562910255543,91.8022376084047,339.539344956919));
#26183=CARTESIAN_POINT('Origin',(203.041252647848,99.3647376084047,339.073593133703));
#26184=CARTESIAN_POINT('',(208.562910255543,90.8022376084047,339.539344956919));
#26185=CARTESIAN_POINT('',(208.562910255543,90.9272376084047,339.539344956919));
#26186=CARTESIAN_POINT('',(208.562910255543,99.3647376084047,339.539344956919));
#26187=CARTESIAN_POINT('Ctrl Pts',(208.562910255543,91.9272376084047,339.539344956919));
#26188=CARTESIAN_POINT('Ctrl Pts',(208.369989533667,91.8647376084047,341.826490424806));
#26189=CARTESIAN_POINT('Ctrl Pts',(206.616317913094,91.8022376084047,343.30733094404));
#26190=CARTESIAN_POINT('Ctrl Pts',(204.86264629252,91.7397376084047,344.788171463274));
#26191=CARTESIAN_POINT('Ctrl Pts',(202.575500824633,91.6772376084047,344.595250741398));
#26192=CARTESIAN_POINT('Ctrl Pts',(200.288355356745,91.6147376084047,344.402330019522));
#26193=CARTESIAN_POINT('Ctrl Pts',(198.807514837511,91.5522376084047,342.648658398949));
#26194=CARTESIAN_POINT('Ctrl Pts',(197.326674318278,91.4897376084047,340.894986778376));
#26195=CARTESIAN_POINT('Ctrl Pts',(197.519595040153,91.4272376084047,338.607841310488));
#26196=CARTESIAN_POINT('Ctrl Pts',(197.712515762029,91.3647376084047,336.320695842601));
#26197=CARTESIAN_POINT('Ctrl Pts',(199.466187382602,91.3022376084047,334.839855323367));
#26198=CARTESIAN_POINT('Ctrl Pts',(201.219859003176,91.2397376084047,333.359014804133));
#26199=CARTESIAN_POINT('Ctrl Pts',(203.507004471063,91.1772376084047,333.551935526009));
#26200=CARTESIAN_POINT('Ctrl Pts',(205.794149938951,91.1147376084047,333.744856247885));
#26201=CARTESIAN_POINT('Ctrl Pts',(207.274990458185,91.0522376084047,335.498527868458));
#26202=CARTESIAN_POINT('Ctrl Pts',(208.755830977418,90.9897376084047,337.252199489031));
#26203=CARTESIAN_POINT('Ctrl Pts',(208.562910255543,90.9272376084047,339.539344956919));
#26204=CARTESIAN_POINT('Ctrl Pts',(208.562910255543,91.8022376084047,339.539344956919));
#26205=CARTESIAN_POINT('Ctrl Pts',(208.369989533667,91.7397376084047,341.826490424806));
#26206=CARTESIAN_POINT('Ctrl Pts',(206.616317913094,91.6772376084047,343.30733094404));
#26207=CARTESIAN_POINT('Ctrl Pts',(204.86264629252,91.6147376084047,344.788171463274));
#26208=CARTESIAN_POINT('Ctrl Pts',(202.575500824633,91.5522376084047,344.595250741398));
#26209=CARTESIAN_POINT('Ctrl Pts',(200.288355356745,91.4897376084047,344.402330019522));
#26210=CARTESIAN_POINT('Ctrl Pts',(198.807514837511,91.4272376084047,342.648658398949));
#26211=CARTESIAN_POINT('Ctrl Pts',(197.326674318278,91.3647376084047,340.894986778376));
#26212=CARTESIAN_POINT('Ctrl Pts',(197.519595040153,91.3022376084047,338.607841310488));
#26213=CARTESIAN_POINT('Ctrl Pts',(197.712515762029,91.2397376084047,336.320695842601));
#26214=CARTESIAN_POINT('Ctrl Pts',(199.466187382602,91.1772376084047,334.839855323367));
#26215=CARTESIAN_POINT('Ctrl Pts',(201.219859003176,91.1147376084047,333.359014804133));
#26216=CARTESIAN_POINT('Ctrl Pts',(203.507004471063,91.0522376084047,333.551935526009));
#26217=CARTESIAN_POINT('Ctrl Pts',(205.794149938951,90.9897376084047,333.744856247885));
#26218=CARTESIAN_POINT('Ctrl Pts',(207.274990458185,90.9272376084047,335.498527868458));
#26219=CARTESIAN_POINT('Ctrl Pts',(208.755830977418,90.8647376084047,337.252199489031));
#26220=CARTESIAN_POINT('Ctrl Pts',(208.562910255543,90.8022376084047,339.539344956919));
#26221=CARTESIAN_POINT('Origin',(203.041252647848,99.3647376084047,339.073593133703));
#26222=CARTESIAN_POINT('',(208.562910255543,89.8022376084047,339.539344956919));
#26223=CARTESIAN_POINT('',(208.562910255543,89.9272376084047,339.539344956919));
#26224=CARTESIAN_POINT('',(208.562910255543,99.3647376084047,339.539344956919));
#26225=CARTESIAN_POINT('',(197.519595040153,89.3022376084047,338.607841310488));
#26226=CARTESIAN_POINT('Ctrl Pts',(208.562910255543,89.8022376084047,339.539344956919));
#26227=CARTESIAN_POINT('Ctrl Pts',(208.369989533667,89.7397376084047,341.826490424806));
#26228=CARTESIAN_POINT('Ctrl Pts',(206.616317913094,89.6772376084047,343.30733094404));
#26229=CARTESIAN_POINT('Ctrl Pts',(204.86264629252,89.6147376084047,344.788171463274));
#26230=CARTESIAN_POINT('Ctrl Pts',(202.575500824633,89.5522376084047,344.595250741398));
#26231=CARTESIAN_POINT('Ctrl Pts',(200.288355356745,89.4897376084047,344.402330019522));
#26232=CARTESIAN_POINT('Ctrl Pts',(198.807514837511,89.4272376084047,342.648658398949));
#26233=CARTESIAN_POINT('Ctrl Pts',(197.326674318278,89.3647376084047,340.894986778376));
#26234=CARTESIAN_POINT('Ctrl Pts',(197.519595040153,89.3022376084047,338.607841310488));
#26235=CARTESIAN_POINT('',(197.519595040153,89.4272376084047,338.607841310488));
#26236=CARTESIAN_POINT('',(197.519595040153,89.3647376084047,338.607841310488));
#26237=CARTESIAN_POINT('Ctrl Pts',(208.562910255543,89.9272376084047,339.539344956919));
#26238=CARTESIAN_POINT('Ctrl Pts',(208.369989533667,89.8647376084047,341.826490424806));
#26239=CARTESIAN_POINT('Ctrl Pts',(206.616317913094,89.8022376084047,343.30733094404));
#26240=CARTESIAN_POINT('Ctrl Pts',(204.86264629252,89.7397376084047,344.788171463274));
#26241=CARTESIAN_POINT('Ctrl Pts',(202.575500824633,89.6772376084047,344.595250741398));
#26242=CARTESIAN_POINT('Ctrl Pts',(200.288355356745,89.6147376084047,344.402330019522));
#26243=CARTESIAN_POINT('Ctrl Pts',(198.807514837511,89.5522376084047,342.648658398949));
#26244=CARTESIAN_POINT('Ctrl Pts',(197.326674318278,89.4897376084046,340.894986778376));
#26245=CARTESIAN_POINT('Ctrl Pts',(197.519595040153,89.4272376084047,338.607841310488));
#26246=CARTESIAN_POINT('Origin',(203.041252647848,90.7397376070391,339.073593133703));
#26247=CARTESIAN_POINT('',(208.023559698486,90.4897376097703,339.49385073704));
#26248=CARTESIAN_POINT('',(208.023559697325,90.2397376062055,339.493850750802));
#26249=CARTESIAN_POINT('',(208.023559698486,90.7397376070391,339.49385073704));
#26250=CARTESIAN_POINT('',(198.05894559721,89.7397376070391,338.653335530367));
#26251=CARTESIAN_POINT('Ctrl Pts',(208.023559697324,90.2397376066219,339.493850750814));
#26252=CARTESIAN_POINT('Ctrl Pts',(207.967987441932,90.2197850692749,340.152680070072));
#26253=CARTESIAN_POINT('Ctrl Pts',(207.782272105817,90.1983863675473,340.794108678668));
#26254=CARTESIAN_POINT('Ctrl Pts',(207.180297127688,90.155775815837,341.951424930312));
#26255=CARTESIAN_POINT('Ctrl Pts',(206.776201966202,90.1349754025954,342.459419328652));
#26256=CARTESIAN_POINT('Ctrl Pts',(205.779186547245,90.0953363464056,343.310258462585));
#26257=CARTESIAN_POINT('Ctrl Pts',(205.189690768065,90.07382879957,343.637577962599));
#26258=CARTESIAN_POINT('Ctrl Pts',(203.940216513502,90.0310110797161,344.033994790525));
#26259=CARTESIAN_POINT('Ctrl Pts',(203.295286092653,90.0102018454483,344.108396766252));
#26260=CARTESIAN_POINT('Ctrl Pts',(201.988697801305,89.970545740923,344.006885610872));
#26261=CARTESIAN_POINT('Ctrl Pts',(201.340411387471,89.9490761928212,343.822541545439));
#26262=CARTESIAN_POINT('Ctrl Pts',(200.175806375358,89.9062643752447,343.221250634602));
#26263=CARTESIAN_POINT('Ctrl Pts',(199.666462394256,89.8854456907724,342.818549125729));
#26264=CARTESIAN_POINT('Ctrl Pts',(198.812968631957,89.8457712813281,341.824314123643));
#26265=CARTESIAN_POINT('Ctrl Pts',(198.484119335941,89.8243423309613,341.236348328231));
#26266=CARTESIAN_POINT('Ctrl Pts',(198.0787326342,89.7810008888298,339.972904723502));
#26267=CARTESIAN_POINT('Ctrl Pts',(198.003482338787,89.7596510109899,339.310872672583));
#26268=CARTESIAN_POINT('Ctrl Pts',(198.05894559721,89.7397376070391,338.653335530367));
#26269=CARTESIAN_POINT('',(198.05894559721,88.9897376097703,338.653335530367));
#26270=CARTESIAN_POINT('',(198.05894559721,89.3647376084047,338.653335530367));
#26271=CARTESIAN_POINT('',(208.023559701634,89.4897376120309,339.493850699717));
#26272=CARTESIAN_POINT('Ctrl Pts',(198.05894559721,88.9897376097702,338.653335530367));
#26273=CARTESIAN_POINT('Ctrl Pts',(198.005090318586,89.0090736882593,339.29180948604));
#26274=CARTESIAN_POINT('Ctrl Pts',(198.074464345089,89.0297695070508,339.934698175558));
#26275=CARTESIAN_POINT('Ctrl Pts',(198.460228811946,89.0725294411995,341.185710855226));
#26276=CARTESIAN_POINT('Ctrl Pts',(198.783316518751,89.0941847312611,341.778563826942));
#26277=CARTESIAN_POINT('Ctrl Pts',(199.626819057716,89.1337898500415,342.782311924146));
#26278=CARTESIAN_POINT('Ctrl Pts',(200.131272251541,89.154503989331,343.190034651175));
#26279=CARTESIAN_POINT('Ctrl Pts',(201.289603850442,89.1973264338864,343.804177733881));
#26280=CARTESIAN_POINT('Ctrl Pts',(201.936946584312,89.2189840397084,343.995714396649));
#26281=CARTESIAN_POINT('Ctrl Pts',(203.242840017277,89.2586049282707,344.110677077451));
#26282=CARTESIAN_POINT('Ctrl Pts',(203.88785366535,89.2792909113593,344.043124405737));
#26283=CARTESIAN_POINT('Ctrl Pts',(205.141524234994,89.3221070406722,343.66003376277));
#26284=CARTESIAN_POINT('Ctrl Pts',(205.735050890444,89.3437671108541,343.338577820788));
#26285=CARTESIAN_POINT('Ctrl Pts',(206.74077207075,89.3834050008466,342.497961995612));
#26286=CARTESIAN_POINT('Ctrl Pts',(207.14975080574,89.4040608004847,341.994741599264));
#26287=CARTESIAN_POINT('Ctrl Pts',(207.766908544629,89.4468700687691,340.838421449675));
#26288=CARTESIAN_POINT('Ctrl Pts',(207.960204977618,89.4685327560788,340.19181273531));
#26289=CARTESIAN_POINT('Ctrl Pts',(208.021696674723,89.4890809562878,339.515515705685));
#26290=CARTESIAN_POINT('Ctrl Pts',(208.022645922154,89.4894095295346,339.504683889451));
#26291=CARTESIAN_POINT('Ctrl Pts',(208.023559701637,89.4897376109016,339.493850699683));
#26292=CARTESIAN_POINT('',(208.023559698486,88.7397376070391,339.49385073704));
#26293=CARTESIAN_POINT('',(208.023559698486,90.7397376070391,339.49385073704));
#26294=CARTESIAN_POINT('Origin',(203.041252647848,88.7397376070391,339.073593133703));
#26295=CARTESIAN_POINT('Ctrl Pts',(208.023559701637,89.4897376109016,339.493850699683));
#26296=CARTESIAN_POINT('Ctrl Pts',(208.076621398869,89.5087887654594,338.864784884326));
#26297=CARTESIAN_POINT('Ctrl Pts',(208.01007822827,89.5291676759465,338.23117685209));
#26298=CARTESIAN_POINT('Ctrl Pts',(207.633971862084,89.5716142611113,336.987154430157));
#26299=CARTESIAN_POINT('Ctrl Pts',(207.31442046961,89.5932797215223,336.392847542905));
#26300=CARTESIAN_POINT('Ctrl Pts',(206.477172736627,89.6329556427219,335.384830836249));
#26301=CARTESIAN_POINT('Ctrl Pts',(205.975388234505,89.6535445750485,334.974388851488));
#26302=CARTESIAN_POINT('Ctrl Pts',(204.821415324561,89.6963382969244,334.353724563616));
#26303=CARTESIAN_POINT('Ctrl Pts',(204.175667351599,89.7180066883986,334.158381533697));
#26304=CARTESIAN_POINT('Ctrl Pts',(202.871295313364,89.7577038137528,334.03538883353));
#26305=CARTESIAN_POINT('Ctrl Pts',(202.226242850506,89.7782558592171,334.098831131073));
#26306=CARTESIAN_POINT('Ctrl Pts',(200.970929427903,89.8210407931791,334.473622444604));
#26307=CARTESIAN_POINT('Ctrl Pts',(200.375722267236,89.8427122741615,334.790956207083));
#26308=CARTESIAN_POINT('Ctrl Pts',(199.365042657244,89.8824321833746,335.624283739083));
#26309=CARTESIAN_POINT('Ctrl Pts',(198.952900510298,89.9029449122807,336.124400305907));
#26310=CARTESIAN_POINT('Ctrl Pts',(198.328169474475,89.9457203070914,337.275640752034));
#26311=CARTESIAN_POINT('Ctrl Pts',(198.130453351107,89.9673950346759,337.920381087117));
#26312=CARTESIAN_POINT('Ctrl Pts',(198.002447617131,90.0071394005659,339.223791172444));
#26313=CARTESIAN_POINT('Ctrl Pts',(198.063325820062,90.0276102965623,339.868868364745));
#26314=CARTESIAN_POINT('Ctrl Pts',(198.432941636231,90.0703753398379,341.125192231522));
#26315=CARTESIAN_POINT('Ctrl Pts',(198.747700402311,90.0920534675672,341.721433688454));
#26316=CARTESIAN_POINT('Ctrl Pts',(199.576477995088,90.1318240574313,342.735191965214));
#26317=CARTESIAN_POINT('Ctrl Pts',(200.074663144713,90.1522505277069,343.149303477133));
#26318=CARTESIAN_POINT('Ctrl Pts',(201.222731634814,90.1950043416697,343.778734947524));
#26319=CARTESIAN_POINT('Ctrl Pts',(201.866294730716,90.2166860169306,343.979193250902));
#26320=CARTESIAN_POINT('Ctrl Pts',(203.168580269176,90.2564846931557,344.112998312768));
#26321=CARTESIAN_POINT('Ctrl Pts',(203.813686573369,90.2768640815098,344.055084606509));
#26322=CARTESIAN_POINT('Ctrl Pts',(205.071164927256,90.319605718618,343.691450627512));
#26323=CARTESIAN_POINT('Ctrl Pts',(205.668588705134,90.3412910795915,343.379672154712));
#26324=CARTESIAN_POINT('Ctrl Pts',(206.685892465735,90.3811197993696,342.556158140771));
#26325=CARTESIAN_POINT('Ctrl Pts',(207.102277090973,90.4014494024921,342.060201444154));
#26326=CARTESIAN_POINT('Ctrl Pts',(207.73712014721,90.444177840985,340.91580305819));
#26327=CARTESIAN_POINT('Ctrl Pts',(207.940734477137,90.465867013117,340.273612075629));
#26328=CARTESIAN_POINT('Ctrl Pts',(208.016544922203,90.4873766903905,339.571581044975));
#26329=CARTESIAN_POINT('Ctrl Pts',(208.020280595153,90.4885602878616,339.532725702126));
#26330=CARTESIAN_POINT('Ctrl Pts',(208.023559698486,90.4897376097703,339.49385073704));
#26331=CARTESIAN_POINT('Origin',(203.041252647848,90.7397376070391,339.073593133703));
#26332=CARTESIAN_POINT('',(208.023559698486,91.4897376097703,339.49385073704));
#26333=CARTESIAN_POINT('',(208.023559700815,91.2397376087116,339.493850709426));
#26334=CARTESIAN_POINT('',(208.023559698486,90.7397376070391,339.49385073704));
#26335=CARTESIAN_POINT('Ctrl Pts',(208.023559700817,91.2397376078761,339.493850709401));
#26336=CARTESIAN_POINT('Ctrl Pts',(208.022777603548,91.2394568054081,339.503122758184));
#26337=CARTESIAN_POINT('Ctrl Pts',(208.021969523626,91.2391756424233,339.512393806923));
#26338=CARTESIAN_POINT('Ctrl Pts',(207.961248460585,91.2186807736327,340.187251224621));
#26339=CARTESIAN_POINT('Ctrl Pts',(207.768528810363,91.1970197338633,340.834101140624));
#26340=CARTESIAN_POINT('Ctrl Pts',(207.152359200336,91.1542061274548,341.991081257056));
#26341=CARTESIAN_POINT('Ctrl Pts',(206.743792353717,91.1335312920547,342.494705903154));
#26342=CARTESIAN_POINT('Ctrl Pts',(205.738717945261,91.0939041360525,343.336268826221));
#26343=CARTESIAN_POINT('Ctrl Pts',(205.145411812608,91.0722456178563,343.658260191733));
#26344=CARTESIAN_POINT('Ctrl Pts',(203.891956933637,91.0294254953918,344.042430123254));
#26345=CARTESIAN_POINT('Ctrl Pts',(203.246948260431,91.0087217510958,344.110517218662));
#26346=CARTESIAN_POINT('Ctrl Pts',(201.94085888431,90.9691108202269,343.996598011257));
#26347=CARTESIAN_POINT('Ctrl Pts',(201.293310661819,90.9474546733328,343.805556421513));
#26348=CARTESIAN_POINT('Ctrl Pts',(200.13441431828,90.9046285537418,343.192261376409));
#26349=CARTESIAN_POINT('Ctrl Pts',(199.629614609139,90.883897862016,342.784891644092));
#26350=CARTESIAN_POINT('Ctrl Pts',(198.785301502277,90.8443019743155,341.781698511198));
#26351=CARTESIAN_POINT('Ctrl Pts',(198.461755707079,90.8226480531073,341.189035529012));
#26352=CARTESIAN_POINT('Ctrl Pts',(198.074450686669,90.7798164147686,339.93620986008));
#26353=CARTESIAN_POINT('Ctrl Pts',(198.004811342931,90.7590606317338,339.291215546541));
#26354=CARTESIAN_POINT('Ctrl Pts',(198.115700527921,90.7194786821743,337.984559478539));
#26355=CARTESIAN_POINT('Ctrl Pts',(198.305303958764,90.6978268463121,337.336416836373));
#26356=CARTESIAN_POINT('Ctrl Pts',(198.9161012012,90.6549925470052,336.175948231855));
#26357=CARTESIAN_POINT('Ctrl Pts',(199.322422686908,90.6342218043809,335.670126393806));
#26358=CARTESIAN_POINT('Ctrl Pts',(200.323893310057,90.5946398319776,334.823555912036));
#26359=CARTESIAN_POINT('Ctrl Pts',(200.915848087721,90.573003751093,334.498699366079));
#26360=CARTESIAN_POINT('Ctrl Pts',(202.167969031834,90.5301668015468,334.108647846274));
#26361=CARTESIAN_POINT('Ctrl Pts',(202.812944576869,90.5093894178012,334.03759841499));
#26362=CARTESIAN_POINT('Ctrl Pts',(204.119678768791,90.4697947026187,334.145756215511));
#26363=CARTESIAN_POINT('Ctrl Pts',(204.767963222047,90.4481874864064,334.333847661661));
#26364=CARTESIAN_POINT('Ctrl Pts',(205.929741942553,90.4053547586586,334.942004109873));
#26365=CARTESIAN_POINT('Ctrl Pts',(206.436569810911,90.3845702374061,335.347297289931));
#26366=CARTESIAN_POINT('Ctrl Pts',(207.285116225065,90.3449618052323,336.346708031024));
#26367=CARTESIAN_POINT('Ctrl Pts',(207.611113328099,90.3233855504265,336.937524743176));
#26368=CARTESIAN_POINT('Ctrl Pts',(208.004111908485,90.2805574126289,338.188423237859));
#26369=CARTESIAN_POINT('Ctrl Pts',(208.076712527105,90.2597652258056,338.833380030691));
#26370=CARTESIAN_POINT('Ctrl Pts',(208.024640833897,90.2401304777962,339.480882387206));
#26371=CARTESIAN_POINT('Ctrl Pts',(208.024106567416,90.2399339536268,339.487367406785));
#26372=CARTESIAN_POINT('Ctrl Pts',(208.023559697324,90.2397376066219,339.493850750815));
#26373=CARTESIAN_POINT('Ctrl Pts',(208.023559698486,90.4897376097703,339.49385073704));
#26374=CARTESIAN_POINT('Ctrl Pts',(208.074141955547,90.5078985499357,338.894179644854));
#26375=CARTESIAN_POINT('Ctrl Pts',(208.016074048837,90.5272800245765,338.289920020022));
#26376=CARTESIAN_POINT('Ctrl Pts',(207.669976465734,90.5687190538142,337.068707858769));
#26377=CARTESIAN_POINT('Ctrl Pts',(207.36163447278,90.5904121457754,336.469940367169));
#26378=CARTESIAN_POINT('Ctrl Pts',(206.544186638362,90.6303071955841,335.448571824803));
#26379=CARTESIAN_POINT('Ctrl Pts',(206.050790454263,90.6505290328337,335.029574160708));
#26380=CARTESIAN_POINT('Ctrl Pts',(204.910622499034,90.6932276895281,334.388528811024));
#26381=CARTESIAN_POINT('Ctrl Pts',(204.270026250128,90.7149247886381,334.181298843545));
#26382=CARTESIAN_POINT('Ctrl Pts',(202.970578181399,90.7548563028777,334.033140891833));
#26383=CARTESIAN_POINT('Ctrl Pts',(202.325397358095,90.7750201800593,334.083725263663));
#26384=CARTESIAN_POINT('Ctrl Pts',(201.065127762074,90.817702082896,334.432579756435));
#26385=CARTESIAN_POINT('Ctrl Pts',(200.464843293427,90.8394032499985,334.736976355467));
#26386=CARTESIAN_POINT('Ctrl Pts',(199.438838548709,90.8793735388622,335.54746334369));
#26387=CARTESIAN_POINT('Ctrl Pts',(199.016851052484,90.8994768022906,336.037931421971));
#26388=CARTESIAN_POINT('Ctrl Pts',(198.368733749474,90.9421405884771,337.173244318086));
#26389=CARTESIAN_POINT('Ctrl Pts',(198.157383424673,90.9638458522645,337.811993279119));
#26390=CARTESIAN_POINT('Ctrl Pts',(198.000468924039,91.0038573003804,339.109672014915));
#26391=CARTESIAN_POINT('Ctrl Pts',(198.046586531689,91.0238973893563,339.754900134417));
#26392=CARTESIAN_POINT('Ctrl Pts',(198.386441780438,91.0665416006326,341.016826928627));
#26393=CARTESIAN_POINT('Ctrl Pts',(198.686331159239,91.0882509514357,341.618810932091));
#26394=CARTESIAN_POINT('Ctrl Pts',(199.488870313868,91.1283060088851,342.650072663083));
#26395=CARTESIAN_POINT('Ctrl Pts',(199.976007972567,91.1482804968743,343.075463033303));
#26396=CARTESIAN_POINT('Ctrl Pts',(201.10577680151,91.1909035761506,343.731596696223));
#26397=CARTESIAN_POINT('Ctrl Pts',(201.74239434411,91.2126169592302,343.947614337832));
#26398=CARTESIAN_POINT('Ctrl Pts',(203.038028984831,91.2527181305916,344.114470201953));
#26399=CARTESIAN_POINT('Ctrl Pts',(203.683312579226,91.2726247708513,344.073419879154));
#26400=CARTESIAN_POINT('Ctrl Pts',(204.947079311213,91.3152250594544,343.743765396875));
#26401=CARTESIAN_POINT('Ctrl Pts',(205.550950855541,91.3369423678553,343.448995896975));
#26402=CARTESIAN_POINT('Ctrl Pts',(206.588133917363,91.3770921991743,342.655480271349));
#26403=CARTESIAN_POINT('Ctrl Pts',(207.01737412275,91.3969289745741,342.17210754058));
#26404=CARTESIAN_POINT('Ctrl Pts',(207.682534559373,91.4395047102744,341.048633463138));
#26405=CARTESIAN_POINT('Ctrl Pts',(207.90380306619,91.4612257773324,340.414463808285));
#26406=CARTESIAN_POINT('Ctrl Pts',(208.006509858919,91.4844128467684,339.668527023477));
#26407=CARTESIAN_POINT('Ctrl Pts',(208.016187834062,91.4870908320957,339.581246876471));
#26408=CARTESIAN_POINT('Ctrl Pts',(208.023559698486,91.4897376097703,339.49385073704));
#26409=CARTESIAN_POINT('Origin',(203.041252647848,90.7397376070391,339.073593133703));
#26410=CARTESIAN_POINT('',(208.023559698486,92.4897376097702,339.49385073704));
#26411=CARTESIAN_POINT('',(208.023559698486,92.2397376070391,339.49385073704));
#26412=CARTESIAN_POINT('',(208.023559698486,90.7397376070391,339.49385073704));
#26413=CARTESIAN_POINT('Ctrl Pts',(208.023559698486,92.2397376070391,339.49385073704));
#26414=CARTESIAN_POINT('Ctrl Pts',(208.020517464755,92.2386453302613,339.529917526663));
#26415=CARTESIAN_POINT('Ctrl Pts',(208.01708222642,92.2375476467766,339.565967592953));
#26416=CARTESIAN_POINT('Ctrl Pts',(207.942746290427,92.2161345415519,340.265432626658));
#26417=CARTESIAN_POINT('Ctrl Pts',(207.740161534077,92.1944477561335,340.908073257731));
#26418=CARTESIAN_POINT('Ctrl Pts',(207.10708409172,92.151710976134,342.053671221179));
#26419=CARTESIAN_POINT('Ctrl Pts',(206.691441794106,92.1313500577135,342.55035555716));
#26420=CARTESIAN_POINT('Ctrl Pts',(205.675294919245,92.0915402777557,343.375589879006));
#26421=CARTESIAN_POINT('Ctrl Pts',(205.078255886551,92.0698572270972,343.688342569117));
#26422=CARTESIAN_POINT('Ctrl Pts',(203.821153157497,92.0271078935813,344.053930965098));
#26423=CARTESIAN_POINT('Ctrl Pts',(203.176056428841,92.0066988775275,344.112813361286));
#26424=CARTESIAN_POINT('Ctrl Pts',(201.873401967365,91.966917911505,343.980903708258));
#26425=CARTESIAN_POINT('Ctrl Pts',(201.229452748241,91.9452384617902,343.781341263561));
#26426=CARTESIAN_POINT('Ctrl Pts',(200.080346273999,91.9024775497843,343.153445553984));
#26427=CARTESIAN_POINT('Ctrl Pts',(199.581529652041,91.8820231121741,342.739977997404));
#26428=CARTESIAN_POINT('Ctrl Pts',(198.751263233901,91.8422690618329,341.727225699921));
#26429=CARTESIAN_POINT('Ctrl Pts',(198.435661751528,91.820593068766,341.131321431086));
#26430=CARTESIAN_POINT('Ctrl Pts',(198.064352892343,91.7778214818585,339.87532692316));
#26431=CARTESIAN_POINT('Ctrl Pts',(198.002635828441,91.7573242411282,339.230257866364));
#26432=CARTESIAN_POINT('Ctrl Pts',(198.129001201107,91.71759530331,337.926531979726));
#26433=CARTESIAN_POINT('Ctrl Pts',(198.325941075757,91.6959226153422,337.281460906651));
#26434=CARTESIAN_POINT('Ctrl Pts',(198.949341762016,91.6531411900911,336.129325382815));
#26435=CARTESIAN_POINT('Ctrl Pts',(199.360927362183,91.6326036927944,335.628662872083));
#26436=CARTESIAN_POINT('Ctrl Pts',(200.370735785543,91.5928981591464,334.794051266812));
#26437=CARTESIAN_POINT('Ctrl Pts',(200.96564898979,91.5712286202447,334.475991011505));
#26438=CARTESIAN_POINT('Ctrl Pts',(202.22067514398,91.5284381304748,334.099738298842));
#26439=CARTESIAN_POINT('Ctrl Pts',(202.865720698403,91.5078628400418,334.035572104211));
#26440=CARTESIAN_POINT('Ctrl Pts',(204.17036252136,91.4681790959201,334.157150043117));
#26441=CARTESIAN_POINT('Ctrl Pts',(204.816393190638,91.4465125479151,334.351822901032));
#26442=CARTESIAN_POINT('Ctrl Pts',(205.971135663743,91.4037137088727,334.971338879327));
#26443=CARTESIAN_POINT('Ctrl Pts',(206.473390617795,91.3831029970338,335.381301410643));
#26444=CARTESIAN_POINT('Ctrl Pts',(207.311742549463,91.3434395197364,336.388566330041));
#26445=CARTESIAN_POINT('Ctrl Pts',(207.631918410012,91.32177580429,336.982618112728));
#26446=CARTESIAN_POINT('Ctrl Pts',(208.009727367198,91.2792733077146,338.227894422968));
#26447=CARTESIAN_POINT('Ctrl Pts',(208.076760034845,91.2588385378259,338.863141318837));
#26448=CARTESIAN_POINT('Ctrl Pts',(208.023559700817,91.2397376078761,339.493850709401));
#26449=CARTESIAN_POINT('Ctrl Pts',(208.023559698486,91.4897376097703,339.49385073704));
#26450=CARTESIAN_POINT('Ctrl Pts',(208.069899534439,91.5063753605728,338.944475093247));
#26451=CARTESIAN_POINT('Ctrl Pts',(208.025106646621,91.524057614868,338.3905838708));
#26452=CARTESIAN_POINT('Ctrl Pts',(207.728366280364,91.5637413335618,337.210042016603));
#26453=CARTESIAN_POINT('Ctrl Pts',(207.439375153272,91.5854659251838,336.604094720386));
#26454=CARTESIAN_POINT('Ctrl Pts',(206.656038908247,91.6257208023941,335.560291864348));
#26455=CARTESIAN_POINT('Ctrl Pts',(206.176893192756,91.6454129861526,335.126725380969));
#26456=CARTESIAN_POINT('Ctrl Pts',(205.060519967291,91.6879339112991,334.451475871497));
#26457=CARTESIAN_POINT('Ctrl Pts',(204.429146484702,91.7096617181724,334.224345307771));
#26458=CARTESIAN_POINT('Ctrl Pts',(203.138553852397,91.7499729797671,334.033716454067));
#26459=CARTESIAN_POINT('Ctrl Pts',(202.493129519806,91.7695911754353,334.062662906401));
#26460=CARTESIAN_POINT('Ctrl Pts',(201.240944432954,91.8115519979504,334.364187588652));
#26461=CARTESIAN_POINT('Ctrl Pts',(200.646587603271,91.832753304877,334.636789266593));
#26462=CARTESIAN_POINT('Ctrl Pts',(199.588991386876,91.8732164414588,335.397844572337));
#26463=CARTESIAN_POINT('Ctrl Pts',(199.137567346313,91.8931225763546,335.881336658372));
#26464=CARTESIAN_POINT('Ctrl Pts',(198.450585441675,91.9355642053956,336.988916328884));
#26465=CARTESIAN_POINT('Ctrl Pts',(198.21927731355,91.9567932396304,337.600944563771));
#26466=CARTESIAN_POINT('Ctrl Pts',(198.002140728478,91.9973185611848,338.885219174848));
#26467=CARTESIAN_POINT('Ctrl Pts',(198.020754761151,92.0171262599735,339.545562830189));
#26468=CARTESIAN_POINT('Ctrl Pts',(198.309989679854,92.0595313129935,340.815939062172));
#26469=CARTESIAN_POINT('Ctrl Pts',(198.575639313402,92.0807885588379,341.4143091349));
#26470=CARTESIAN_POINT('Ctrl Pts',(199.323444141224,92.121378160502,342.48019223246));
#26471=CARTESIAN_POINT('Ctrl Pts',(199.800000993709,92.1410879524949,342.936405838262));
#26472=CARTESIAN_POINT('Ctrl Pts',(200.897816914169,92.1834538593166,343.637236510666));
#26473=CARTESIAN_POINT('Ctrl Pts',(201.507624368599,92.2047396824536,343.876631250823));
#26474=CARTESIAN_POINT('Ctrl Pts',(202.788192744678,92.2453955333451,344.109648388601));
#26475=CARTESIAN_POINT('Ctrl Pts',(203.446952875112,92.265008647927,344.099656435787));
#26476=CARTESIAN_POINT('Ctrl Pts',(204.72027149577,92.3073327523818,343.827813912942));
#26477=CARTESIAN_POINT('Ctrl Pts',(205.322915410455,92.3286473876907,343.569787711577));
#26478=CARTESIAN_POINT('Ctrl Pts',(206.397717593833,92.3693713073093,342.836425211467));
#26479=CARTESIAN_POINT('Ctrl Pts',(206.859090121511,92.3888897174023,342.367358322678));
#26480=CARTESIAN_POINT('Ctrl Pts',(207.574810597222,92.4311692919078,341.280209575513));
#26481=CARTESIAN_POINT('Ctrl Pts',(207.822934129627,92.4525128324795,340.672922664461));
#26482=CARTESIAN_POINT('Ctrl Pts',(207.983048828277,92.4786231563991,339.855911999456));
#26483=CARTESIAN_POINT('Ctrl Pts',(208.008263172363,92.4842455793272,339.675196629055));
#26484=CARTESIAN_POINT('Ctrl Pts',(208.023559698486,92.4897376097703,339.49385073704));
#26485=CARTESIAN_POINT('Origin',(203.041252647848,90.7397376070391,339.073593133703));
#26486=CARTESIAN_POINT('',(208.023559698486,93.4897376097702,339.49385073704));
#26487=CARTESIAN_POINT('',(208.023559698486,93.2397376070391,339.49385073704));
#26488=CARTESIAN_POINT('',(208.023559698486,90.7397376070391,339.49385073704));
#26489=CARTESIAN_POINT('Ctrl Pts',(208.023559698486,93.2397376070391,339.49385073704));
#26490=CARTESIAN_POINT('Ctrl Pts',(208.016584375434,93.2372332026896,339.576545733987));
#26491=CARTESIAN_POINT('Ctrl Pts',(208.007544240813,93.2347008137002,339.659138336034));
#26492=CARTESIAN_POINT('Ctrl Pts',(207.907560317782,93.211676921936,340.400858899981));
#26493=CARTESIAN_POINT('Ctrl Pts',(207.687990813611,93.1899581719302,341.035826439867));
#26494=CARTESIAN_POINT('Ctrl Pts',(207.025752146929,93.1473669371886,342.161344020006));
#26495=CARTESIAN_POINT('Ctrl Pts',(206.597760178299,93.1274864417577,342.645937109802));
#26496=CARTESIAN_POINT('Ctrl Pts',(205.562493897218,93.0873672065052,343.442382086359));
#26497=CARTESIAN_POINT('Ctrl Pts',(204.959230218942,93.0656523263478,343.73881395107));
#26498=CARTESIAN_POINT('Ctrl Pts',(203.696055976313,93.0230376480925,344.071778028136));
#26499=CARTESIAN_POINT('Ctrl Pts',(203.050790602721,93.0030885138555,344.114472922847));
#26500=CARTESIAN_POINT('Ctrl Pts',(201.754488251591,92.9630163493192,343.95084432293));
#26501=CARTESIAN_POINT('Ctrl Pts',(201.117174804287,92.9413054676046,343.736340576226));
#26502=CARTESIAN_POINT('Ctrl Pts',(199.985602468861,92.8986690434082,343.08280780898));
#26503=CARTESIAN_POINT('Ctrl Pts',(199.497382928909,92.8786534365176,342.658523124953));
#26504=CARTESIAN_POINT('Ctrl Pts',(198.692258383647,92.8386258208235,341.628967190428));
#26505=CARTESIAN_POINT('Ctrl Pts',(198.390902569519,92.8169190111372,341.027532231744));
#26506=CARTESIAN_POINT('Ctrl Pts',(198.048121398057,92.7742624361431,339.766140737552));
#26507=CARTESIAN_POINT('Ctrl Pts',(198.000551155381,92.7541827208717,339.120928161138));
#26508=CARTESIAN_POINT('Ctrl Pts',(198.154617219303,92.7141971819735,337.822670682765));
#26509=CARTESIAN_POINT('Ctrl Pts',(198.364628162582,92.6924944701812,337.183317717646));
#26510=CARTESIAN_POINT('Ctrl Pts',(199.010446143125,92.6498192395829,336.04642260089));
#26511=CARTESIAN_POINT('Ctrl Pts',(199.431460314172,92.6296779310761,335.55500148697));
#26512=CARTESIAN_POINT('Ctrl Pts',(200.455957517435,92.5897320584838,334.742246118233));
#26513=CARTESIAN_POINT('Ctrl Pts',(201.055750561644,92.5680334296138,334.436563575521));
#26514=CARTESIAN_POINT('Ctrl Pts',(202.315540845168,92.5253409418072,334.085138141637));
#26515=CARTESIAN_POINT('Ctrl Pts',(202.96070842996,92.5051406632066,334.033278261959));
#26516=CARTESIAN_POINT('Ctrl Pts',(204.260656162087,92.4652321176993,334.178936982935));
#26517=CARTESIAN_POINT('Ctrl Pts',(204.901774474389,92.4435375223459,334.384989397671));
#26518=CARTESIAN_POINT('Ctrl Pts',(206.043323261248,92.4008290825914,335.024014436143));
#26519=CARTESIAN_POINT('Ctrl Pts',(206.537554260903,92.3805725266765,335.442160013568));
#26520=CARTESIAN_POINT('Ctrl Pts',(207.356982019679,92.3406990481215,336.4622043698));
#26521=CARTESIAN_POINT('Ctrl Pts',(207.666445831867,92.3190084083253,337.060535513476));
#26522=CARTESIAN_POINT('Ctrl Pts',(208.015499581875,92.2774682195176,338.284055932193));
#26523=CARTESIAN_POINT('Ctrl Pts',(208.07438933635,92.2579873662533,338.891246855278));
#26524=CARTESIAN_POINT('Ctrl Pts',(208.023559698486,92.239737607039,339.49385073704));
#26525=CARTESIAN_POINT('Ctrl Pts',(208.023559698486,92.4897376097703,339.49385073704));
#26526=CARTESIAN_POINT('Ctrl Pts',(208.062763029538,92.503813085854,339.029080959744));
#26527=CARTESIAN_POINT('Ctrl Pts',(208.036816019941,92.5186621687676,338.560218780518));
#26528=CARTESIAN_POINT('Ctrl Pts',(207.819237647414,92.5549651861974,337.463074845365));
#26529=CARTESIAN_POINT('Ctrl Pts',(207.56949024203,92.576337573963,336.855936542507));
#26530=CARTESIAN_POINT('Ctrl Pts',(206.85171428554,92.6172023755726,335.771639663891));
#26531=CARTESIAN_POINT('Ctrl Pts',(206.390651310047,92.6365404256281,335.304767332239));
#26532=CARTESIAN_POINT('Ctrl Pts',(205.315040387593,92.6787225624914,334.573212485897));
#26533=CARTESIAN_POINT('Ctrl Pts',(204.710587265591,92.7001235808703,334.315769800306));
#26534=CARTESIAN_POINT('Ctrl Pts',(203.438632779674,92.74106078414,334.047312375077));
#26535=CARTESIAN_POINT('Ctrl Pts',(202.783410504634,92.7603147840207,334.038225280269));
#26536=CARTESIAN_POINT('Ctrl Pts',(201.504028352964,92.8024439697371,334.271393146257));
#26537=CARTESIAN_POINT('Ctrl Pts',(200.892227160201,92.8238732386862,334.512245249282));
#26538=CARTESIAN_POINT('Ctrl Pts',(199.797940959952,92.8648838432939,335.213378888698));
#26539=CARTESIAN_POINT('Ctrl Pts',(199.325269217626,92.8840589473803,335.665985013689));
#26540=CARTESIAN_POINT('Ctrl Pts',(198.577071554176,92.9261323728689,336.729251978811));
#26541=CARTESIAN_POINT('Ctrl Pts',(198.309796155385,92.9475893466673,337.330553540224));
#26542=CARTESIAN_POINT('Ctrl Pts',(198.022018744288,92.9886741004599,338.597611461723));
#26543=CARTESIAN_POINT('Ctrl Pts',(198.002619168953,93.007776237796,339.250907302441));
#26544=CARTESIAN_POINT('Ctrl Pts',(198.214788436499,93.0497911379274,340.53331005053));
#26545=CARTESIAN_POINT('Ctrl Pts',(198.446192384073,93.0712751059638,341.149880227393));
#26546=CARTESIAN_POINT('Ctrl Pts',(199.129759078033,93.1124344915023,342.254546141058));
#26547=CARTESIAN_POINT('Ctrl Pts',(199.573536121332,93.131470324171,342.733263264169));
#26548=CARTESIAN_POINT('Ctrl Pts',(200.623751002207,93.173424007641,343.498738697488));
#26549=CARTESIAN_POINT('Ctrl Pts',(201.221590068503,93.194934098379,343.776259350343));
#26550=CARTESIAN_POINT('Ctrl Pts',(202.483388821072,93.2361683229841,344.084186720265));
#26551=CARTESIAN_POINT('Ctrl Pts',(203.134680304963,93.2551451870716,344.114280628453));
#26552=CARTESIAN_POINT('Ctrl Pts',(204.420025246542,93.2970350674323,343.923946124849));
#26553=CARTESIAN_POINT('Ctrl Pts',(205.04140056564,93.3185702556276,343.702454501577));
#26554=CARTESIAN_POINT('Ctrl Pts',(206.156712318979,93.3598792453007,343.037206727527));
#26555=CARTESIAN_POINT('Ctrl Pts',(206.64165617648,93.3788050750477,342.602532781206));
#26556=CARTESIAN_POINT('Ctrl Pts',(207.424839088953,93.4206287022077,341.56594739536));
#26557=CARTESIAN_POINT('Ctrl Pts',(207.712895253196,93.4421878193285,340.971861730333));
#26558=CARTESIAN_POINT('Ctrl Pts',(207.951094625822,93.4721791769352,340.061455246487));
#26559=CARTESIAN_POINT('Ctrl Pts',(207.999539074984,93.4811132989645,339.778623982982));
#26560=CARTESIAN_POINT('Ctrl Pts',(208.023559698486,93.4897376097702,339.49385073704));
#26561=CARTESIAN_POINT('Origin',(203.041252647848,90.7397376070391,339.073593133703));
#26562=CARTESIAN_POINT('',(208.023559698486,94.4897376097702,339.49385073704));
#26563=CARTESIAN_POINT('',(208.023559698486,94.239737607039,339.49385073704));
#26564=CARTESIAN_POINT('',(208.023559698486,90.7397376070391,339.49385073704));
#26565=CARTESIAN_POINT('Ctrl Pts',(208.023559698486,94.2397376070391,339.49385073704));
#26566=CARTESIAN_POINT('Ctrl Pts',(208.010416806229,94.2350188124707,339.649664514677));
#26567=CARTESIAN_POINT('Ctrl Pts',(207.989949726939,94.2302028827843,339.805041669434));
#26568=CARTESIAN_POINT('Ctrl Pts',(207.847186504248,94.2050486441458,340.598070875467));
#26569=CARTESIAN_POINT('Ctrl Pts',(207.609006140685,94.1837711461655,341.208218819053));
#26570=CARTESIAN_POINT('Ctrl Pts',(206.910251725032,94.1413936065866,342.30750821154));
#26571=CARTESIAN_POINT('Ctrl Pts',(206.45475666335,94.1216554905342,342.785106712135));
#26572=CARTESIAN_POINT('Ctrl Pts',(205.390116506321,94.0810847559065,343.534909180295));
#26573=CARTESIAN_POINT('Ctrl Pts',(204.79234583872,94.0598357420271,343.801609538172));
#26574=CARTESIAN_POINT('Ctrl Pts',(203.52238779423,94.0174198117079,344.093253090569));
#26575=CARTESIAN_POINT('Ctrl Pts',(202.861825332427,93.997583565249,344.113063442553));
#26576=CARTESIAN_POINT('Ctrl Pts',(201.562180369908,93.9566078398427,343.895636535585));
#26577=CARTESIAN_POINT('Ctrl Pts',(200.93639988694,93.9348726148643,343.657184900668));
#26578=CARTESIAN_POINT('Ctrl Pts',(199.833965931474,93.8924634819524,342.962410051128));
#26579=CARTESIAN_POINT('Ctrl Pts',(199.363060303142,93.8730223740733,342.520397591058));
#26580=CARTESIAN_POINT('Ctrl Pts',(198.599711326465,93.8325669773609,341.463781129068));
#26581=CARTESIAN_POINT('Ctrl Pts',(198.322071276732,93.8108332685872,340.853922978363));
#26582=CARTESIAN_POINT('Ctrl Pts',(198.026390289346,93.7683883495924,339.584320308703));
#26583=CARTESIAN_POINT('Ctrl Pts',(198.002254957477,93.7488728393059,338.938836700015));
#26584=CARTESIAN_POINT('Ctrl Pts',(198.202341366308,93.7084797670189,337.65031087724));
#26585=CARTESIAN_POINT('Ctrl Pts',(198.433873038498,93.6867481919507,337.021081219462));
#26586=CARTESIAN_POINT('Ctrl Pts',(199.116706243766,93.6442697891709,335.910091099344));
#26587=CARTESIAN_POINT('Ctrl Pts',(199.553541446658,93.6246796835069,335.434136338493));
#26588=CARTESIAN_POINT('Ctrl Pts',(200.602320962549,93.5843464794912,334.658517829307));
#26589=CARTESIAN_POINT('Ctrl Pts',(201.209804236407,93.5626175563798,334.373909121373));
#26590=CARTESIAN_POINT('Ctrl Pts',(202.47709123836,93.5201078798684,334.064434339146));
#26591=CARTESIAN_POINT('Ctrl Pts',(203.122490723531,93.5004435265117,334.033423393591));
#26592=CARTESIAN_POINT('Ctrl Pts',(204.413959289153,93.4601676700277,334.219995156549));
#26593=CARTESIAN_POINT('Ctrl Pts',(205.046242389075,93.4384418242896,334.445234179375));
#26594=CARTESIAN_POINT('Ctrl Pts',(206.164915447719,93.3959029861141,335.117226760056));
#26595=CARTESIAN_POINT('Ctrl Pts',(206.64542795061,93.3761652142158,335.54939389652));
#26596=CARTESIAN_POINT('Ctrl Pts',(207.432061201653,93.3359441439206,336.591059618701));
#26597=CARTESIAN_POINT('Ctrl Pts',(207.722924153347,93.3142217152644,337.196340812184));
#26598=CARTESIAN_POINT('Ctrl Pts',(208.024304415469,93.274367399161,338.380885456566));
#26599=CARTESIAN_POINT('Ctrl Pts',(208.070307946708,93.2565219932672,338.939633216943));
#26600=CARTESIAN_POINT('Ctrl Pts',(208.023559698486,93.239737607039,339.49385073704));
#26601=CARTESIAN_POINT('Ctrl Pts',(208.023559698486,93.4897376097703,339.49385073704));
#26602=CARTESIAN_POINT('Ctrl Pts',(208.053467706927,93.5004757140647,339.13928039698));
#26603=CARTESIAN_POINT('Ctrl Pts',(208.045509564255,93.5116822219815,338.781728251426));
#26604=CARTESIAN_POINT('Ctrl Pts',(207.914698776637,93.5442095446849,337.778250092893));
#26605=CARTESIAN_POINT('Ctrl Pts',(207.703471833047,93.565791292366,337.152107083396));
#26606=CARTESIAN_POINT('Ctrl Pts',(207.057085527107,93.6072484595061,336.026022407149));
#26607=CARTESIAN_POINT('Ctrl Pts',(206.631676783548,93.6260979455809,335.534743749621));
#26608=CARTESIAN_POINT('Ctrl Pts',(205.609138567905,93.6677824164138,334.733651852745));
#26609=CARTESIAN_POINT('Ctrl Pts',(205.019063155191,93.6893853826483,334.434908324653));
#26610=CARTESIAN_POINT('Ctrl Pts',(203.768687207825,93.7309154070329,334.085139839588));
#26611=CARTESIAN_POINT('Ctrl Pts',(203.121532565595,93.7497402717904,334.033019530661));
#26612=CARTESIAN_POINT('Ctrl Pts',(201.830736440786,93.7913522630566,334.17823605667));
#26613=CARTESIAN_POINT('Ctrl Pts',(201.199936002383,93.8129749406107,334.378976721327));
#26614=CARTESIAN_POINT('Ctrl Pts',(200.063097911448,93.8545766580724,335.006197099869));
#26615=CARTESIAN_POINT('Ctrl Pts',(199.565455788559,93.8733861699124,335.422298491117));
#26616=CARTESIAN_POINT('Ctrl Pts',(198.746493044917,93.9149240864483,336.430554314477));
#26617=CARTESIAN_POINT('Ctrl Pts',(198.43705788505,93.9365648914709,337.016410161944));
#26618=CARTESIAN_POINT('Ctrl Pts',(198.066138750965,93.9782368879476,338.260751574102));
#26619=CARTESIAN_POINT('Ctrl Pts',(198.002966642329,93.9970403544056,338.905830082094));
#26620=CARTESIAN_POINT('Ctrl Pts',(198.125493048056,94.0385028711359,340.199055243097));
#26621=CARTESIAN_POINT('Ctrl Pts',(198.315669239932,94.0601601685294,340.83433527832));
#26622=CARTESIAN_POINT('Ctrl Pts',(198.923674631269,94.1019007900959,341.981760995852));
#26623=CARTESIAN_POINT('Ctrl Pts',(199.33054862406,94.1207074421516,342.485713525102));
#26624=CARTESIAN_POINT('Ctrl Pts',(200.32448278348,94.1620935167283,343.322270439877));
#26625=CARTESIAN_POINT('Ctrl Pts',(200.90596895485,94.1837656404107,343.64225289854));
#26626=CARTESIAN_POINT('Ctrl Pts',(202.14416501544,94.2255730245481,344.034097997918));
#26627=CARTESIAN_POINT('Ctrl Pts',(202.787202018954,94.2443918735921,344.108157061287));
#26628=CARTESIAN_POINT('Ctrl Pts',(204.082621116741,94.2857007687482,344.008001235342));
#26629=CARTESIAN_POINT('Ctrl Pts',(204.722144944031,94.3073860438215,343.828319305139));
#26630=CARTESIAN_POINT('Ctrl Pts',(205.879852883803,94.3492581431384,343.23931938036));
#26631=CARTESIAN_POINT('Ctrl Pts',(206.38998517162,94.3680978628903,342.8414728654));
#26632=CARTESIAN_POINT('Ctrl Pts',(207.243633680452,94.4093291548137,341.861702064357));
#26633=CARTESIAN_POINT('Ctrl Pts',(207.573877783122,94.4310259190769,341.284668113954));
#26634=CARTESIAN_POINT('Ctrl Pts',(207.909525740834,94.4651666382827,340.281623235055));
#26635=CARTESIAN_POINT('Ctrl Pts',(207.990143356593,94.4777398812994,339.890013648779));
#26636=CARTESIAN_POINT('Ctrl Pts',(208.023559698486,94.4897376097703,339.49385073704));
#26637=CARTESIAN_POINT('Origin',(203.041252647848,90.7397376070391,339.073593133703));
#26638=CARTESIAN_POINT('',(208.023559698486,95.4897376097703,339.49385073704));
#26639=CARTESIAN_POINT('',(208.023559698486,95.239737607039,339.49385073704));
#26640=CARTESIAN_POINT('',(208.023559698486,90.7397376070391,339.49385073704));
#26641=CARTESIAN_POINT('Ctrl Pts',(208.023559698486,95.239737607039,339.49385073704));
#26642=CARTESIAN_POINT('Ctrl Pts',(208.002184735619,95.2320631882956,339.747258711949));
#26643=CARTESIAN_POINT('Ctrl Pts',(207.961461981359,95.224140643241,339.99922146964));
#26644=CARTESIAN_POINT('Ctrl Pts',(207.748241493299,95.1953258739236,340.881988667412));
#26645=CARTESIAN_POINT('Ctrl Pts',(207.472228860018,95.1738232666891,341.480348925067));
#26646=CARTESIAN_POINT('Ctrl Pts',(206.709292797331,95.1318515425915,342.532497335783));
#26647=CARTESIAN_POINT('Ctrl Pts',(206.231465939511,95.1127971911816,342.977575255451));
#26648=CARTESIAN_POINT('Ctrl Pts',(205.1283260951,95.0716595022217,343.663742642687));
#26649=CARTESIAN_POINT('Ctrl Pts',(204.512452008966,95.0501832868781,343.896548980516));
#26650=CARTESIAN_POINT('Ctrl Pts',(203.230484038253,95.008151117896,344.111823287934));
#26651=CARTESIAN_POINT('Ctrl Pts',(202.576903215927,94.989028455691,344.093946787673));
#26652=CARTESIAN_POINT('Ctrl Pts',(201.309111357273,94.9479652863878,343.80902975649));
#26653=CARTESIAN_POINT('Ctrl Pts',(200.70733281563,94.9265162883599,343.543209633316));
#26654=CARTESIAN_POINT('Ctrl Pts',(199.642227731743,94.8844263903836,342.797471251603));
#26655=CARTESIAN_POINT('Ctrl Pts',(199.188369040292,94.8652289627601,342.32565784608));
#26656=CARTESIAN_POINT('Ctrl Pts',(198.484759138229,94.8242397523614,341.232848339848));
#26657=CARTESIAN_POINT('Ctrl Pts',(198.2425799626,94.8028186346644,340.621732038546));
#26658=CARTESIAN_POINT('Ctrl Pts',(198.006447420102,94.7606737885907,339.342791610849));
#26659=CARTESIAN_POINT('Ctrl Pts',(198.01407610868,94.7413958878486,338.687297565162));
#26660=CARTESIAN_POINT('Ctrl Pts',(198.279810342739,94.7004798138802,337.414664330447));
#26661=CARTESIAN_POINT('Ctrl Pts',(198.535866571647,94.6790870740884,336.809780215669));
#26662=CARTESIAN_POINT('Ctrl Pts',(199.265069544064,94.6368900963985,335.73244288771));
#26663=CARTESIAN_POINT('Ctrl Pts',(199.73112397612,94.6175267983182,335.270188525124));
#26664=CARTESIAN_POINT('Ctrl Pts',(200.814010005854,94.5766827909723,334.5500824108));
#26665=CARTESIAN_POINT('Ctrl Pts',(201.420484220555,94.5553187613266,334.299094057792));
#26666=CARTESIAN_POINT('Ctrl Pts',(202.696379945475,94.5130724765636,334.043182426579));
#26667=CARTESIAN_POINT('Ctrl Pts',(203.353685010861,94.4936196597669,334.041064225867));
#26668=CARTESIAN_POINT('Ctrl Pts',(204.630767916029,94.4528464191918,334.288658157108));
#26669=CARTESIAN_POINT('Ctrl Pts',(205.238439837012,94.4315112696395,334.535476741688));
#26670=CARTESIAN_POINT('Ctrl Pts',(206.32719185158,94.3892184852296,335.248974915445));
#26671=CARTESIAN_POINT('Ctrl Pts',(206.797378841282,94.3696728341906,335.709576758465));
#26672=CARTESIAN_POINT('Ctrl Pts',(207.532909923555,94.3289688501493,336.783047182977));
#26673=CARTESIAN_POINT('Ctrl Pts',(207.792083799821,94.3076625940288,337.385056061122));
#26674=CARTESIAN_POINT('Ctrl Pts',(208.033463659016,94.2704276874328,338.50455736156));
#26675=CARTESIAN_POINT('Ctrl Pts',(208.065101493989,94.254652680156,339.00135761143));
#26676=CARTESIAN_POINT('Ctrl Pts',(208.023559698486,94.239737607039,339.49385073704));
#26677=CARTESIAN_POINT('Ctrl Pts',(208.023559698486,94.4897376097702,339.49385073704));
#26678=CARTESIAN_POINT('Ctrl Pts',(208.043768367793,94.4969932850888,339.254269597342));
#26679=CARTESIAN_POINT('Ctrl Pts',(208.046713370765,94.504471619991,339.013036344154));
#26680=CARTESIAN_POINT('Ctrl Pts',(207.992401460983,94.5329829269995,338.11421889948));
#26681=CARTESIAN_POINT('Ctrl Pts',(207.822998666388,94.5546895512273,337.470732835158));
#26682=CARTESIAN_POINT('Ctrl Pts',(207.252545517764,94.5966843279668,336.303171643436));
#26683=CARTESIAN_POINT('Ctrl Pts',(206.863417586195,94.6155899329068,335.787063449034));
#26684=CARTESIAN_POINT('Ctrl Pts',(205.897461723054,94.6566660118852,334.917026478739));
#26685=CARTESIAN_POINT('Ctrl Pts',(205.324890950684,94.6783809183672,334.576932970826));
#26686=CARTESIAN_POINT('Ctrl Pts',(204.098967452958,94.7204334190671,334.144982523275));
#26687=CARTESIAN_POINT('Ctrl Pts',(203.45980384356,94.7393828773307,334.050170387513));
#26688=CARTESIAN_POINT('Ctrl Pts',(202.160744370393,94.7803819694335,334.107672237849));
#26689=CARTESIAN_POINT('Ctrl Pts',(201.513609429568,94.8021036483627,334.267144490897));
#26690=CARTESIAN_POINT('Ctrl Pts',(200.336726746597,94.844211349363,334.819735997519));
#26691=CARTESIAN_POINT('Ctrl Pts',(199.814910653824,94.8632110439442,335.200548522953));
#26692=CARTESIAN_POINT('Ctrl Pts',(198.929355509185,94.9041339614367,336.153209740886));
#26693=CARTESIAN_POINT('Ctrl Pts',(198.579930763012,94.9258609848434,336.721377403406));
#26694=CARTESIAN_POINT('Ctrl Pts',(198.129264059369,94.9680213100446,337.9413473242));
#26695=CARTESIAN_POINT('Ctrl Pts',(198.02480881621,94.9870768938179,338.578721474358));
#26696=CARTESIAN_POINT('Ctrl Pts',(198.062504346938,95.0279247298472,339.879233592402));
#26697=CARTESIAN_POINT('Ctrl Pts',(198.212509986815,95.0496557628878,340.529686371043));
#26698=CARTESIAN_POINT('Ctrl Pts',(198.748118246612,95.0918661086761,341.715280275465));
#26699=CARTESIAN_POINT('Ctrl Pts',(199.121094664281,95.1109824755923,342.242483631134));
#26700=CARTESIAN_POINT('Ctrl Pts',(200.061127156013,95.1517565849168,343.142558313204));
#26701=CARTESIAN_POINT('Ctrl Pts',(200.625017830817,95.1734903944396,343.500714594113));
#26702=CARTESIAN_POINT('Ctrl Pts',(201.839260640202,95.2157481529159,343.96896608168));
#26703=CARTESIAN_POINT('Ctrl Pts',(202.474963975221,95.2349294259626,344.082461960223));
#26704=CARTESIAN_POINT('Ctrl Pts',(203.776702189642,95.2756314027013,344.063317889121));
#26705=CARTESIAN_POINT('Ctrl Pts',(204.430137152372,95.2973668631158,343.922222439557));
#26706=CARTESIAN_POINT('Ctrl Pts',(205.623779055288,95.3396694432978,343.402566090827));
#26707=CARTESIAN_POINT('Ctrl Pts',(206.156009434055,95.3589189781057,343.036890373666));
#26708=CARTESIAN_POINT('Ctrl Pts',(207.069517447052,95.3995506311888,342.108706580024));
#26709=CARTESIAN_POINT('Ctrl Pts',(207.435749836129,95.4212867277573,341.548909322898));
#26710=CARTESIAN_POINT('Ctrl Pts',(207.867118588414,95.458981461004,340.47284835785));
#26711=CARTESIAN_POINT('Ctrl Pts',(207.981927662159,95.4747901367899,339.987413700515));
#26712=CARTESIAN_POINT('Ctrl Pts',(208.023559698486,95.4897376097703,339.49385073704));
#26713=CARTESIAN_POINT('Origin',(203.041252647848,90.7397376070391,339.073593133703));
#26714=CARTESIAN_POINT('',(208.023559698486,96.4897376097702,339.49385073704));
#26715=CARTESIAN_POINT('',(208.023559698486,96.2397376070391,339.49385073704));
#26716=CARTESIAN_POINT('',(208.023559698486,90.7397376070391,339.49385073704));
#26717=CARTESIAN_POINT('Ctrl Pts',(208.023559698486,96.239737607039,339.49385073704));
#26718=CARTESIAN_POINT('Ctrl Pts',(207.992788965512,96.2286897520627,339.858648990853));
#26719=CARTESIAN_POINT('Ctrl Pts',(207.92197943703,96.2171481933558,340.219775056907));
#26720=CARTESIAN_POINT('Ctrl Pts',(207.615114011323,96.1841690870811,341.197661696786));
#26721=CARTESIAN_POINT('Ctrl Pts',(207.296647798149,96.1625010943826,341.779788832638));
#26722=CARTESIAN_POINT('Ctrl Pts',(206.462618291474,96.12109274177,342.775796357516));
#26723=CARTESIAN_POINT('Ctrl Pts',(205.959575321926,96.1022879546357,343.183999868238));
#26724=CARTESIAN_POINT('Ctrl Pts',(204.813670409927,96.0605670693968,343.794787058174));
#26725=CARTESIAN_POINT('Ctrl Pts',(204.179027129829,96.0389143884731,343.986495650469));
#26726=CARTESIAN_POINT('Ctrl Pts',(202.886140400462,95.9974298653367,344.112302424058));
#26727=CARTESIAN_POINT('Ctrl Pts',(202.240762010827,95.9786256015654,344.050727383065));
#26728=CARTESIAN_POINT('Ctrl Pts',(200.995535928686,95.9369738439711,343.682870646351));
#26729=CARTESIAN_POINT('Ctrl Pts',(200.409056860537,95.9153381342076,343.374981703873));
#26730=CARTESIAN_POINT('Ctrl Pts',(199.398721120808,95.8737785691662,342.558601039208));
#26731=CARTESIAN_POINT('Ctrl Pts',(198.981270905831,95.8549655572264,342.061880964911));
#26732=CARTESIAN_POINT('Ctrl Pts',(198.351259785361,95.8133845163022,340.926596740914));
#26733=CARTESIAN_POINT('Ctrl Pts',(198.148988889215,95.7917674001189,340.296462727989));
#26734=CARTESIAN_POINT('Ctrl Pts',(198.000470813963,95.7501341935238,339.006037204878));
#26735=CARTESIAN_POINT('Ctrl Pts',(198.050981883652,95.7313031343742,338.358580322264));
#26736=CARTESIAN_POINT('Ctrl Pts',(198.397679001331,95.689794148103,337.107342611361));
#26737=CARTESIAN_POINT('Ctrl Pts',(198.694867641288,95.6681971894426,336.516670935736));
#26738=CARTESIAN_POINT('Ctrl Pts',(199.493357025268,95.6264920180173,335.492074911149));
#26739=CARTESIAN_POINT('Ctrl Pts',(199.983712583493,95.6076336653908,335.065315997816));
#26740=CARTESIAN_POINT('Ctrl Pts',(201.108231479152,95.5661978288938,334.416167513942));
#26741=CARTESIAN_POINT('Ctrl Pts',(201.733687698866,95.5446225092986,334.203433823101));
#26742=CARTESIAN_POINT('Ctrl Pts',(203.021447045494,95.5028473003782,334.032234906729));
#26743=CARTESIAN_POINT('Ctrl Pts',(203.670982588125,95.4839525958251,334.071680876363));
#26744=CARTESIAN_POINT('Ctrl Pts',(204.928029241843,95.442590742841,334.397319762798));
#26745=CARTESIAN_POINT('Ctrl Pts',(205.522676538958,95.4210384431454,334.683834055209));
#26746=CARTESIAN_POINT('Ctrl Pts',(206.561269974001,95.3791953419735,335.464428959567));
#26747=CARTESIAN_POINT('Ctrl Pts',(206.997277895647,95.3602555477126,335.948460603411));
#26748=CARTESIAN_POINT('Ctrl Pts',(207.665223302619,95.3189682353603,337.062216008946));
#26749=CARTESIAN_POINT('Ctrl Pts',(207.88817825794,95.297440217797,337.682894516322));
#26750=CARTESIAN_POINT('Ctrl Pts',(208.043677427071,95.2637698364477,338.715232680993));
#26751=CARTESIAN_POINT('Ctrl Pts',(208.056256739997,95.2514770795136,339.106215393474));
#26752=CARTESIAN_POINT('Ctrl Pts',(208.023559698486,95.239737607039,339.49385073704));
#26753=CARTESIAN_POINT('Ctrl Pts',(208.023559698486,95.4897376097703,339.49385073704));
#26754=CARTESIAN_POINT('Ctrl Pts',(208.035542263805,95.4940398031565,339.351793058128));
#26755=CARTESIAN_POINT('Ctrl Pts',(208.041462561782,95.4984229426763,339.209066621738));
#26756=CARTESIAN_POINT('Ctrl Pts',(208.040247657829,95.523515304071,338.403183597517));
#26757=CARTESIAN_POINT('Ctrl Pts',(207.907438736615,95.5452511338183,337.747095622329));
#26758=CARTESIAN_POINT('Ctrl Pts',(207.402593756487,95.5876357444217,336.546097118296));
#26759=CARTESIAN_POINT('Ctrl Pts',(207.043647495372,95.6070289008787,336.009226080566));
#26760=CARTESIAN_POINT('Ctrl Pts',(206.126452073802,95.6475260610186,335.083418894112));
#26761=CARTESIAN_POINT('Ctrl Pts',(205.570518321967,95.669260831511,334.709796433752));
#26762=CARTESIAN_POINT('Ctrl Pts',(204.366807565089,95.7116827696874,334.21020725588));
#26763=CARTESIAN_POINT('Ctrl Pts',(203.734057619306,95.7311498865385,334.080636839829));
#26764=CARTESIAN_POINT('Ctrl Pts',(202.430459439187,95.7715831732276,334.066857680717));
#26765=CARTESIAN_POINT('Ctrl Pts',(201.772032500655,95.7933161995137,334.192045533994));
#26766=CARTESIAN_POINT('Ctrl Pts',(200.564374593779,95.8357731071012,334.683285324514));
#26767=CARTESIAN_POINT('Ctrl Pts',(200.023262402187,95.8553147591124,335.036090056167));
#26768=CARTESIAN_POINT('Ctrl Pts',(199.086302193444,95.8956865729828,335.943204405379));
#26769=CARTESIAN_POINT('Ctrl Pts',(198.705983574932,95.9174172730076,336.495538568604));
#26770=CARTESIAN_POINT('Ctrl Pts',(198.192743707955,95.9599068792456,337.694528949623));
#26771=CARTESIAN_POINT('Ctrl Pts',(198.056182177743,95.9795230633547,338.326001488763));
#26772=CARTESIAN_POINT('Ctrl Pts',(198.028116087924,96.019835886017,339.63028254547));
#26773=CARTESIAN_POINT('Ctrl Pts',(198.146366380844,96.0415637748267,340.290755597831));
#26774=CARTESIAN_POINT('Ctrl Pts',(198.625232381097,96.08408390344,341.504388797045));
#26775=CARTESIAN_POINT('Ctrl Pts',(198.972483193822,96.1037740964638,342.049341216364));
#26776=CARTESIAN_POINT('Ctrl Pts',(199.870440162225,96.1440304655269,342.996326912094));
#26777=CARTESIAN_POINT('Ctrl Pts',(200.419460273735,96.1657551485722,343.382659145238));
#26778=CARTESIAN_POINT('Ctrl Pts',(201.614125354356,96.2083037228219,343.908204657125));
#26779=CARTESIAN_POINT('Ctrl Pts',(202.244450704624,96.2280669411377,344.051064528939));
#26780=CARTESIAN_POINT('Ctrl Pts',(203.549282441482,96.268269426818,344.091981841699));
#26781=CARTESIAN_POINT('Ctrl Pts',(204.211533659972,96.2899905926433,343.979988270638));
#26782=CARTESIAN_POINT('Ctrl Pts',(205.430486009242,96.3325656385476,343.51227456024));
#26783=CARTESIAN_POINT('Ctrl Pts',(205.97888624372,96.3524004981135,343.170004557191));
#26784=CARTESIAN_POINT('Ctrl Pts',(206.934812909489,96.3925516816892,342.280291170605));
#26785=CARTESIAN_POINT('Ctrl Pts',(207.326502801641,96.4142690942686,341.734289428821));
#26786=CARTESIAN_POINT('Ctrl Pts',(207.832866129487,96.454472222825,340.610535606034));
#26787=CARTESIAN_POINT('Ctrl Pts',(207.975973891469,96.4726525083101,340.057997821903));
#26788=CARTESIAN_POINT('Ctrl Pts',(208.023559698486,96.4897376097703,339.49385073704));
#26789=CARTESIAN_POINT('Origin',(203.041252647848,90.7397376070391,339.073593133703));
#26790=CARTESIAN_POINT('',(208.023559698486,97.4897376097703,339.49385073704));
#26791=CARTESIAN_POINT('',(208.023559698486,97.239737607039,339.49385073704));
#26792=CARTESIAN_POINT('',(208.023559698486,90.7397376070391,339.49385073704));
#26793=CARTESIAN_POINT('',(203.461510341368,97.739737607039,334.091286090672));
#26794=CARTESIAN_POINT('Ctrl Pts',(208.023559698486,97.4897376097703,339.49385073704));
#26795=CARTESIAN_POINT('Ctrl Pts',(208.026122456743,97.4906577367488,339.463468303909));
#26796=CARTESIAN_POINT('Ctrl Pts',(208.028408300908,97.4915817077204,339.43305061537));
#26797=CARTESIAN_POINT('Ctrl Pts',(208.074332770675,97.5127995193416,338.736640391277));
#26798=CARTESIAN_POINT('Ctrl Pts',(207.984466746736,97.5344812925574,338.06860228078));
#26799=CARTESIAN_POINT('Ctrl Pts',(207.5561645317,97.5772347898467,336.831354383881));
#26800=CARTESIAN_POINT('Ctrl Pts',(207.231321281585,97.5976600214372,336.270864071329));
#26801=CARTESIAN_POINT('Ctrl Pts',(206.370658555201,97.6374313462935,335.284041543343));
#26802=CARTESIAN_POINT('Ctrl Pts',(205.835545208142,97.6591095681029,334.873889238233));
#26803=CARTESIAN_POINT('Ctrl Pts',(204.679764352328,97.7011145474933,334.309334586702));
#26804=CARTESIAN_POINT('Ctrl Pts',(204.078139965998,97.7210630803458,334.143298811198));
#26805=CARTESIAN_POINT('Ctrl Pts',(203.461510341367,97.739737607039,334.091286090672));
#26806=CARTESIAN_POINT('',(198.05894559721,97.739737607039,338.653335530367));
#26807=CARTESIAN_POINT('Origin',(203.041252647848,97.739737607039,339.073593133703));
#26808=CARTESIAN_POINT('Ctrl Pts',(198.05894559721,97.739737607039,338.653335530367));
#26809=CARTESIAN_POINT('Ctrl Pts',(198.108214107373,97.7220483516143,338.069239386452));
#26810=CARTESIAN_POINT('Ctrl Pts',(198.259812626742,97.7032083417734,337.498354791864));
#26811=CARTESIAN_POINT('Ctrl Pts',(198.755574421492,97.6648102145717,336.431322092174));
#26812=CARTESIAN_POINT('Ctrl Pts',(199.097269421509,97.6455484329761,335.944110190914));
#26813=CARTESIAN_POINT('Ctrl Pts',(199.969816698936,97.607292294862,335.076622710325));
#26814=CARTESIAN_POINT('Ctrl Pts',(200.506038837376,97.5879204097589,334.716736066367));
#26815=CARTESIAN_POINT('Ctrl Pts',(201.70601300298,97.5455470870172,334.209815220194));
#26816=CARTESIAN_POINT('Ctrl Pts',(202.361735860209,97.5238110933426,334.075844224131));
#26817=CARTESIAN_POINT('Ctrl Pts',(203.664358449214,97.4832281495198,334.071475003247));
#26818=CARTESIAN_POINT('Ctrl Pts',(204.298734616266,97.4639285428047,334.192179097569));
#26819=CARTESIAN_POINT('Ctrl Pts',(205.508309937176,97.4215957040894,334.674473301726));
#26820=CARTESIAN_POINT('Ctrl Pts',(206.068687981791,97.3998596942166,335.039575687551));
#26821=CARTESIAN_POINT('Ctrl Pts',(206.998539556133,97.3592078266473,335.95120373491));
#26822=CARTESIAN_POINT('Ctrl Pts',(207.365240030686,97.3399784069158,336.482728028812));
#26823=CARTESIAN_POINT('Ctrl Pts',(207.887142855589,97.2976885717295,337.675244394378));
#26824=CARTESIAN_POINT('Ctrl Pts',(208.029494077743,97.2759534810375,338.328267227807));
#26825=CARTESIAN_POINT('Ctrl Pts',(208.043369207323,97.2499792315604,339.158452004541));
#26826=CARTESIAN_POINT('Ctrl Pts',(208.037667377192,97.244802796371,339.326599064431));
#26827=CARTESIAN_POINT('Ctrl Pts',(208.023559698486,97.2397376070391,339.49385073704));
#26828=CARTESIAN_POINT('Origin',(203.041252647848,90.7397376070391,339.073593133703));
#26829=CARTESIAN_POINT('Ctrl Pts',(208.023559698486,97.2397376070391,339.49385073704));
#26830=CARTESIAN_POINT('Ctrl Pts',(207.984072407315,97.2255601785509,339.961986965035));
#26831=CARTESIAN_POINT('Ctrl Pts',(207.878733270431,97.2106005068773,340.423058333001));
#26832=CARTESIAN_POINT('Ctrl Pts',(207.473249346603,97.1738244260834,341.480836170954));
#26833=CARTESIAN_POINT('Ctrl Pts',(207.116320666296,97.1520913016813,342.045337432396));
#26834=CARTESIAN_POINT('Ctrl Pts',(206.218287475554,97.1112959462238,342.987156700394));
#26835=CARTESIAN_POINT('Ctrl Pts',(205.691844425507,97.0921976813484,343.361238276784));
#26836=CARTESIAN_POINT('Ctrl Pts',(204.507474627792,97.0500015858584,343.899250516616));
#26837=CARTESIAN_POINT('Ctrl Pts',(203.857482527551,97.0282715850081,344.05059746488));
#26838=CARTESIAN_POINT('Ctrl Pts',(202.557166736546,96.9874020839181,344.091093101459));
#26839=CARTESIAN_POINT('Ctrl Pts',(201.919539958598,96.9683632608377,343.988001630071));
#26840=CARTESIAN_POINT('Ctrl Pts',(200.698718343136,96.9262179431037,343.539984552674));
#26841=CARTESIAN_POINT('Ctrl Pts',(200.129917988798,96.9044923291968,343.19187851264));
#26842=CARTESIAN_POINT('Ctrl Pts',(199.175365484415,96.8635474014795,342.308516192129));
#26843=CARTESIAN_POINT('Ctrl Pts',(198.793374274254,96.8445629039893,341.787509714422));
#26844=CARTESIAN_POINT('Ctrl Pts',(198.238240806987,96.8024709621138,340.611943598142));
#26845=CARTESIAN_POINT('Ctrl Pts',(198.077353598602,96.7807510980283,339.965317957328));
#26846=CARTESIAN_POINT('Ctrl Pts',(198.016882311117,96.7397297302301,338.666489160782));
#26847=CARTESIAN_POINT('Ctrl Pts',(198.110249291279,96.720793689799,338.027056762429));
#26848=CARTESIAN_POINT('Ctrl Pts',(198.539398866779,96.6787576872925,336.800254802914));
#26849=CARTESIAN_POINT('Ctrl Pts',(198.878092804007,96.6570450260351,336.227038361008));
#26850=CARTESIAN_POINT('Ctrl Pts',(199.745801725264,96.6159464905269,335.259105973311));
#26851=CARTESIAN_POINT('Ctrl Pts',(200.261057849086,96.5970523201022,334.868735662898));
#26852=CARTESIAN_POINT('Ctrl Pts',(201.427219829101,96.5550747605428,334.295628248824));
#26853=CARTESIAN_POINT('Ctrl Pts',(202.070149690122,96.5333708331789,334.124752260644));
#26854=CARTESIAN_POINT('Ctrl Pts',(203.367247441408,96.4921947026469,334.043247659781));
#26855=CARTESIAN_POINT('Ctrl Pts',(204.008587493501,96.4733351478506,334.12638067621));
#26856=CARTESIAN_POINT('Ctrl Pts',(205.241507999327,96.4314184484144,334.53572903349));
#26857=CARTESIAN_POINT('Ctrl Pts',(205.81919049922,96.4097248493973,334.86450662431));
#26858=CARTESIAN_POINT('Ctrl Pts',(206.800999585091,96.3684710070079,335.715713801429));
#26859=CARTESIAN_POINT('Ctrl Pts',(207.200139551435,96.349638214465,336.224960207563));
#26860=CARTESIAN_POINT('Ctrl Pts',(207.791875026247,96.3077846788651,337.381199760928));
#26861=CARTESIAN_POINT('Ctrl Pts',(207.973070003739,96.2861030489872,338.02012421056));
#26862=CARTESIAN_POINT('Ctrl Pts',(208.04718331331,96.2564700331562,338.948673262516));
#26863=CARTESIAN_POINT('Ctrl Pts',(208.046467436216,96.2479623498323,339.222271157521));
#26864=CARTESIAN_POINT('Ctrl Pts',(208.023559698486,96.2397376070391,339.49385073704));
#26865=CARTESIAN_POINT('Ctrl Pts',(208.023559698486,96.4897376097703,339.49385073704));
#26866=CARTESIAN_POINT('Ctrl Pts',(208.029723508158,96.4919506501753,339.42077652697));
#26867=CARTESIAN_POINT('Ctrl Pts',(208.034284582085,96.494185613006,339.347508739407));
#26868=CARTESIAN_POINT('Ctrl Pts',(208.063924596539,96.516875971816,338.608972787657));
#26869=CARTESIAN_POINT('Ctrl Pts',(207.957526488708,96.5385894627631,337.945184750735));
#26870=CARTESIAN_POINT('Ctrl Pts',(207.499782065111,96.581211947686,336.721530599689));
#26871=CARTESIAN_POINT('Ctrl Pts',(207.161945349506,96.6011846285669,336.17005856649));
#26872=CARTESIAN_POINT('Ctrl Pts',(206.279592795086,96.6412409005394,335.206214374461));
#26873=CARTESIAN_POINT('Ctrl Pts',(205.736313511846,96.6629503613836,334.809785055021));
#26874=CARTESIAN_POINT('Ctrl Pts',(204.549100349265,96.7055940218374,334.263472632413));
#26875=CARTESIAN_POINT('Ctrl Pts',(203.920702461476,96.7256323670771,334.109989051609));
#26876=CARTESIAN_POINT('Ctrl Pts',(202.615078789907,96.7656449626129,334.047443538443));
#26877=CARTESIAN_POINT('Ctrl Pts',(201.949968540392,96.787350337298,334.148875006118));
#26878=CARTESIAN_POINT('Ctrl Pts',(200.722184066173,96.8300136134775,334.597772957799));
#26879=CARTESIAN_POINT('Ctrl Pts',(200.167994064226,96.8501152007867,334.931690311607));
#26880=CARTESIAN_POINT('Ctrl Pts',(199.197182607504,96.8900865715947,335.807517898597));
#26881=CARTESIAN_POINT('Ctrl Pts',(198.796587014991,96.9117878493224,336.348362849379));
#26882=CARTESIAN_POINT('Ctrl Pts',(198.241665087836,96.9544692803354,337.532429750623));
#26883=CARTESIAN_POINT('Ctrl Pts',(198.083778098994,96.9746315520822,338.160031382078));
#26884=CARTESIAN_POINT('Ctrl Pts',(198.012287620772,97.0145640846887,339.4659334706));
#26885=CARTESIAN_POINT('Ctrl Pts',(198.109339878621,97.0362612931975,340.13217709862));
#26886=CARTESIAN_POINT('Ctrl Pts',(198.550438928581,97.0789595137171,341.36357013281));
#26887=CARTESIAN_POINT('Ctrl Pts',(198.880912065787,97.0991798182293,341.920150291995));
#26888=CARTESIAN_POINT('Ctrl Pts',(199.750992859848,97.1390758249433,342.897058847645));
#26889=CARTESIAN_POINT('Ctrl Pts',(200.289677786506,97.1607690242843,343.301296724813));
#26890=CARTESIAN_POINT('Ctrl Pts',(201.470958966748,97.2034827607414,343.863765735229));
#26891=CARTESIAN_POINT('Ctrl Pts',(202.097863816094,97.2237583890752,344.025512719996));
#26892=CARTESIAN_POINT('Ctrl Pts',(203.403986190896,97.2636201008004,344.104834054828));
#26893=CARTESIAN_POINT('Ctrl Pts',(204.071198444298,97.2853093776467,344.011620455692));
#26894=CARTESIAN_POINT('Ctrl Pts',(205.305729222954,97.3280374440981,343.57735712454));
#26895=CARTESIAN_POINT('Ctrl Pts',(205.864399867483,97.3483656623101,343.249894588557));
#26896=CARTESIAN_POINT('Ctrl Pts',(206.846618092953,97.3881952230552,342.384846483844));
#26897=CARTESIAN_POINT('Ctrl Pts',(207.254024869897,97.4098806855625,341.848065254827));
#26898=CARTESIAN_POINT('Ctrl Pts',(207.809808680381,97.451625474599,340.696719088236));
#26899=CARTESIAN_POINT('Ctrl Pts',(207.972228684743,97.4713078376846,340.102398612571));
#26900=CARTESIAN_POINT('Ctrl Pts',(208.023559698486,97.4897376097703,339.49385073704));
#26901=CARTESIAN_POINT('Origin',(203.041252647848,90.7397376070391,339.073593133703));
#26902=CARTESIAN_POINT('',(213.005866749124,88.7397376070391,339.914108340376));
#26903=CARTESIAN_POINT('Origin',(203.041252647848,88.7397376070391,339.073593133703));
#26904=CARTESIAN_POINT('',(213.005866749124,90.7397376070391,339.914108340376));
#26905=CARTESIAN_POINT('',(213.005866749124,90.7397376070391,339.914108340376));
#26906=CARTESIAN_POINT('Origin',(203.041252647848,90.7397376070391,339.073593133703));
#26907=CARTESIAN_POINT('Origin',(203.041252647848,97.739737607039,339.073593133703));
#26908=CARTESIAN_POINT('',(199.42962580375,97.739737607039,347.299137232417));
#26909=CARTESIAN_POINT('',(205.224003640602,97.739737607039,347.787893007159));
#26910=CARTESIAN_POINT('',(197.436702983495,97.739737607039,347.131034191082));
#26911=CARTESIAN_POINT('',(208.358969375234,97.739737607039,346.314125779038));
#26912=CARTESIAN_POINT('',(206.791486507918,97.739737607039,347.051009393099));
#26913=CARTESIAN_POINT('',(211.679433210834,97.739737607039,341.54042526057));
#26914=CARTESIAN_POINT('',(207.216926460858,97.739737607039,347.955996048494));
#26915=CARTESIAN_POINT('',(211.970596219332,97.739737607039,338.088581680325));
#26916=CARTESIAN_POINT('',(211.825014715083,97.739737607039,339.814503470448));
#26917=CARTESIAN_POINT('',(209.496682218079,97.739737607039,332.826125387114));
#26918=CARTESIAN_POINT('',(212.82147612521,97.739737607039,339.898554991115));
#26919=CARTESIAN_POINT('',(206.652879491945,97.7397376070391,330.84804903499));
#26920=CARTESIAN_POINT('',(208.074780855012,97.739737607039,331.837087211052));
#26921=CARTESIAN_POINT('',(200.858501655094,97.7397376070391,330.359293260247));
#26922=CARTESIAN_POINT('',(208.645802312201,97.7397376070391,331.016152076324));
#26923=CARTESIAN_POINT('',(197.723535920462,97.739737607039,331.833060488368));
#26924=CARTESIAN_POINT('',(199.291018787778,97.7397376070391,331.096176874308));
#26925=CARTESIAN_POINT('',(194.403072084862,97.739737607039,336.606761006836));
#26926=CARTESIAN_POINT('',(198.865578834838,97.7397376070391,330.191190218913));
#26927=CARTESIAN_POINT('',(194.111909076364,97.739737607039,340.058604587082));
#26928=CARTESIAN_POINT('',(194.257490580613,97.739737607039,338.332682796959));
#26929=CARTESIAN_POINT('',(196.585823077617,97.739737607039,345.321060880292));
#26930=CARTESIAN_POINT('',(193.261029170486,97.739737607039,338.248631276292));
#26931=CARTESIAN_POINT('',(198.007724440684,97.739737607039,346.310099056355));
#26932=CARTESIAN_POINT('Ctrl Pts',(204.724000912662,97.739737607039,344.353175103396));
#26933=CARTESIAN_POINT('Ctrl Pts',(204.228206354228,97.739737607039,344.483763605689));
#26934=CARTESIAN_POINT('Ctrl Pts',(203.716680544754,97.7397376070576,344.544816894783));
#26935=CARTESIAN_POINT('Ctrl Pts',(202.823445454301,97.7397376070576,344.527012055876));
#26936=CARTESIAN_POINT('Ctrl Pts',(202.280691335722,97.7397376070391,344.478986669827));
#26937=CARTESIAN_POINT('Ctrl Pts',(200.995881515023,97.7397376070391,344.06556316677));
#26938=CARTESIAN_POINT('Ctrl Pts',(200.383354713341,97.7397376070391,343.725835780105));
#26939=CARTESIAN_POINT('Ctrl Pts',(199.471189684133,97.7397376070391,342.955161691881));
#26940=CARTESIAN_POINT('Ctrl Pts',(198.962966730132,97.7397376070398,342.435039038614));
#26941=CARTESIAN_POINT('Ctrl Pts',(198.336602864625,97.7397376070398,341.211676486358));
#26942=CARTESIAN_POINT('Ctrl Pts',(198.172351502433,97.739737607039,340.718613950579));
#26943=CARTESIAN_POINT('Ctrl Pts',(197.977751507247,97.739737607039,339.584101577175));
#26944=CARTESIAN_POINT('Ctrl Pts',(198.004985132087,97.739737607039,339.046563828707));
#26945=CARTESIAN_POINT('Ctrl Pts',(198.05894559721,97.739737607039,338.653335530367));
#26946=CARTESIAN_POINT('Ctrl Pts',(203.461510341368,97.739737607039,334.091286090672));
#26947=CARTESIAN_POINT('Ctrl Pts',(203.984159147494,97.739737607039,334.107979462843));
#26948=CARTESIAN_POINT('Ctrl Pts',(204.501119720434,97.739737607039,334.204906851929));
#26949=CARTESIAN_POINT('Ctrl Pts',(205.482808994414,97.739737607039,334.550879748362));
#26950=CARTESIAN_POINT('Ctrl Pts',(205.94223007391,97.7397376070383,334.796447456792));
#26951=CARTESIAN_POINT('Ctrl Pts',(207.010186372729,97.7397376070383,335.596363647632));
#26952=CARTESIAN_POINT('Ctrl Pts',(207.443993549644,97.739737607039,336.165426518184));
#26953=CARTESIAN_POINT('Ctrl Pts',(208.075942876397,97.739737607039,337.239425210693));
#26954=CARTESIAN_POINT('Ctrl Pts',(208.307395377785,97.739737607039,337.900716986882));
#26955=CARTESIAN_POINT('Ctrl Pts',(208.478391743638,97.739737607039,339.100710339751));
#26956=CARTESIAN_POINT('Ctrl Pts',(208.47697792236,97.7397376070082,339.621944596309));
#26957=CARTESIAN_POINT('Ctrl Pts',(208.32126756147,97.7397376070082,340.658543246856));
#26958=CARTESIAN_POINT('Ctrl Pts',(208.175600019025,97.739737607039,341.151251001225));
#26959=CARTESIAN_POINT('Ctrl Pts',(207.964363569528,97.739737607039,341.616938637223));
#26960=CARTESIAN_POINT('Origin',(203.041252647848,90.7397376070391,339.073593133703));
#26961=CARTESIAN_POINT('',(197.436702983495,90.7397376070391,347.131034191082));
#26962=CARTESIAN_POINT('',(207.216926460858,90.7397376070391,347.955996048494));
#26963=CARTESIAN_POINT('',(197.436702983495,90.7397376070391,347.131034191082));
#26964=CARTESIAN_POINT('',(193.261029170486,90.7397376070391,338.248631276292));
#26965=CARTESIAN_POINT('',(193.261029170486,90.7397376070391,338.248631276292));
#26966=CARTESIAN_POINT('',(198.865578834838,90.7397376070391,330.191190218913));
#26967=CARTESIAN_POINT('',(198.865578834838,90.7397376070391,330.191190218913));
#26968=CARTESIAN_POINT('',(208.645802312201,90.7397376070391,331.016152076324));
#26969=CARTESIAN_POINT('',(208.645802312201,90.7397376070391,331.016152076324));
#26970=CARTESIAN_POINT('',(212.82147612521,90.7397376070391,339.898554991115));
#26971=CARTESIAN_POINT('',(212.82147612521,90.7397376070391,339.898554991115));
#26972=CARTESIAN_POINT('',(207.216926460858,90.7397376070391,347.955996048494));
#26973=CARTESIAN_POINT('Origin',(203.041252647848,88.7397376070391,339.073593133703));
#26974=CARTESIAN_POINT('Origin',(197.436702983495,97.739737607039,347.131034191082));
#26975=CARTESIAN_POINT('',(207.216926460858,95.7397376070391,347.955996048494));
#26976=CARTESIAN_POINT('',(201.330353312049,101.647214895151,347.459463599121));
#26977=CARTESIAN_POINT('',(197.436702983495,95.7397376070391,347.131034191082));
#26978=CARTESIAN_POINT('',(198.433164393623,96.739737607039,347.21508571175));
#26979=CARTESIAN_POINT('',(197.436702983495,97.739737607039,347.131034191082));
#26980=CARTESIAN_POINT('',(207.216926460858,97.739737607039,347.955996048494));
#26981=CARTESIAN_POINT('Origin',(207.216926460858,97.739737607039,347.955996048494));
#26982=CARTESIAN_POINT('',(207.787947918046,96.7397376070391,347.135060913766));
#26983=CARTESIAN_POINT('',(212.82147612521,95.7397376070391,339.898554991115));
#26984=CARTESIAN_POINT('',(212.82147612521,97.739737607039,339.898554991115));
#26985=CARTESIAN_POINT('',(209.448179835846,101.647214895151,344.748210654532));
#26986=CARTESIAN_POINT('Origin',(212.82147612521,97.739737607039,339.898554991115));
#26987=CARTESIAN_POINT('',(208.645802312201,95.7397376070391,331.016152076324));
#26988=CARTESIAN_POINT('',(211.159079171645,101.647214895151,336.362340189115));
#26989=CARTESIAN_POINT('',(212.396036172271,96.739737607039,338.99356833572));
#26990=CARTESIAN_POINT('',(208.645802312201,97.7397376070391,331.016152076324));
#26991=CARTESIAN_POINT('Origin',(208.645802312201,97.7397376070391,331.016152076324));
#26992=CARTESIAN_POINT('',(207.649340902073,96.7397376070391,330.932100555657));
#26993=CARTESIAN_POINT('',(198.865578834838,95.7397376070391,330.191190218913));
#26994=CARTESIAN_POINT('',(198.865578834838,97.7397376070391,330.191190218913));
#26995=CARTESIAN_POINT('',(204.752151983647,101.647214895151,330.687722668286));
#26996=CARTESIAN_POINT('Origin',(198.865578834838,97.7397376070391,330.191190218913));
#26997=CARTESIAN_POINT('',(193.261029170486,95.7397376070391,338.248631276292));
#26998=CARTESIAN_POINT('',(196.63432545985,101.647214895151,333.398975612875));
#26999=CARTESIAN_POINT('',(198.29455737765,96.7397376070391,331.012125353641));
#27000=CARTESIAN_POINT('',(193.261029170486,97.739737607039,338.248631276292));
#27001=CARTESIAN_POINT('Origin',(193.261029170486,97.739737607039,338.248631276292));
#27002=CARTESIAN_POINT('',(194.923426124051,101.647214895151,341.784846078292));
#27003=CARTESIAN_POINT('',(193.686469123425,96.739737607039,339.153617931687));
#27004=CARTESIAN_POINT('Origin',(197.519595040153,89.3647376084047,338.607841310488));
#27005=CARTESIAN_POINT('',(197.789270318682,89.1459876090874,338.630588420428));
#27006=CARTESIAN_POINT('',(197.789270318682,89.5834876077218,338.630588420428));
#27007=CARTESIAN_POINT('Origin',(203.041252647848,99.3647376084047,339.073593133703));
#27008=CARTESIAN_POINT('Ctrl Pts',(208.562910255543,90.9272376084047,339.539344956919));
#27009=CARTESIAN_POINT('Ctrl Pts',(208.369989533667,90.8647376084047,341.826490424806));
#27010=CARTESIAN_POINT('Ctrl Pts',(206.616317913094,90.8022376084047,343.30733094404));
#27011=CARTESIAN_POINT('Ctrl Pts',(204.86264629252,90.7397376084047,344.788171463274));
#27012=CARTESIAN_POINT('Ctrl Pts',(202.575500824633,90.6772376084047,344.595250741398));
#27013=CARTESIAN_POINT('Ctrl Pts',(200.288355356745,90.6147376084047,344.402330019522));
#27014=CARTESIAN_POINT('Ctrl Pts',(198.807514837511,90.5522376084047,342.648658398949));
#27015=CARTESIAN_POINT('Ctrl Pts',(197.326674318278,90.4897376084047,340.894986778376));
#27016=CARTESIAN_POINT('Ctrl Pts',(197.519595040153,90.4272376084047,338.607841310488));
#27017=CARTESIAN_POINT('Ctrl Pts',(197.712515762029,90.3647376084047,336.320695842601));
#27018=CARTESIAN_POINT('Ctrl Pts',(199.466187382602,90.3022376084047,334.839855323367));
#27019=CARTESIAN_POINT('Ctrl Pts',(201.219859003176,90.2397376084047,333.359014804133));
#27020=CARTESIAN_POINT('Ctrl Pts',(203.507004471063,90.1772376084047,333.551935526009));
#27021=CARTESIAN_POINT('Ctrl Pts',(205.794149938951,90.1147376084047,333.744856247885));
#27022=CARTESIAN_POINT('Ctrl Pts',(207.274990458185,90.0522376084047,335.498527868458));
#27023=CARTESIAN_POINT('Ctrl Pts',(208.755830977418,89.9897376084047,337.252199489031));
#27024=CARTESIAN_POINT('Ctrl Pts',(208.562910255543,89.9272376084047,339.539344956919));
#27025=CARTESIAN_POINT('Ctrl Pts',(208.562910255543,90.8022376084047,339.539344956919));
#27026=CARTESIAN_POINT('Ctrl Pts',(208.369989533667,90.7397376084047,341.826490424806));
#27027=CARTESIAN_POINT('Ctrl Pts',(206.616317913094,90.6772376084047,343.30733094404));
#27028=CARTESIAN_POINT('Ctrl Pts',(204.86264629252,90.6147376084047,344.788171463274));
#27029=CARTESIAN_POINT('Ctrl Pts',(202.575500824633,90.5522376084047,344.595250741398));
#27030=CARTESIAN_POINT('Ctrl Pts',(200.288355356745,90.4897376084047,344.402330019522));
#27031=CARTESIAN_POINT('Ctrl Pts',(198.807514837511,90.4272376084047,342.648658398949));
#27032=CARTESIAN_POINT('Ctrl Pts',(197.326674318278,90.3647376084047,340.894986778376));
#27033=CARTESIAN_POINT('Ctrl Pts',(197.519595040153,90.3022376084047,338.607841310488));
#27034=CARTESIAN_POINT('Ctrl Pts',(197.712515762029,90.2397376084047,336.320695842601));
#27035=CARTESIAN_POINT('Ctrl Pts',(199.466187382602,90.1772376084047,334.839855323367));
#27036=CARTESIAN_POINT('Ctrl Pts',(201.219859003176,90.1147376084047,333.359014804133));
#27037=CARTESIAN_POINT('Ctrl Pts',(203.507004471063,90.0522376084047,333.551935526009));
#27038=CARTESIAN_POINT('Ctrl Pts',(205.794149938951,89.9897376084047,333.744856247885));
#27039=CARTESIAN_POINT('Ctrl Pts',(207.274990458185,89.9272376084047,335.498527868458));
#27040=CARTESIAN_POINT('Ctrl Pts',(208.755830977418,89.8647376084047,337.252199489031));
#27041=CARTESIAN_POINT('Ctrl Pts',(208.562910255543,89.8022376084047,339.539344956919));
#27042=CARTESIAN_POINT('Ctrl Pts',(198.05894559721,99.7397376070391,338.653335530367));
#27043=CARTESIAN_POINT('Ctrl Pts',(198.233021996202,99.677237607039,336.589596378086));
#27044=CARTESIAN_POINT('Ctrl Pts',(199.815396547552,99.614737607039,335.253403031079));
#27045=CARTESIAN_POINT('Ctrl Pts',(201.397771098903,99.5522376070391,333.917209684073));
#27046=CARTESIAN_POINT('Ctrl Pts',(203.461510251184,99.4897376070391,334.091286083065));
#27047=CARTESIAN_POINT('Ctrl Pts',(205.525249403466,99.4272376070391,334.265362482058));
#27048=CARTESIAN_POINT('Ctrl Pts',(206.861442750472,99.364737607039,335.847737033408));
#27049=CARTESIAN_POINT('Ctrl Pts',(208.197636097478,99.3022376070391,337.430111584758));
#27050=CARTESIAN_POINT('Ctrl Pts',(208.023559698486,99.239737607039,339.49385073704));
#27051=CARTESIAN_POINT('Ctrl Pts',(207.849483299494,99.1772376070391,341.557589889321));
#27052=CARTESIAN_POINT('Ctrl Pts',(206.267108748143,99.1147376070391,342.893783236327));
#27053=CARTESIAN_POINT('Ctrl Pts',(204.684734196793,99.0522376070391,344.229976583334));
#27054=CARTESIAN_POINT('Ctrl Pts',(202.620995044512,98.989737607039,344.055900184342));
#27055=CARTESIAN_POINT('Ctrl Pts',(200.55725589223,98.9272376070391,343.881823785349));
#27056=CARTESIAN_POINT('Ctrl Pts',(199.221062545224,98.8647376070391,342.299449233999));
#27057=CARTESIAN_POINT('Ctrl Pts',(197.884869198218,98.8022376070391,340.717074682649));
#27058=CARTESIAN_POINT('Ctrl Pts',(198.05894559721,98.739737607039,338.653335530367));
#27059=CARTESIAN_POINT('Ctrl Pts',(198.233021996202,98.6772376070391,336.589596378086));
#27060=CARTESIAN_POINT('Ctrl Pts',(199.815396547552,98.6147376070391,335.253403031079));
#27061=CARTESIAN_POINT('Ctrl Pts',(201.397771098903,98.5522376070391,333.917209684073));
#27062=CARTESIAN_POINT('Ctrl Pts',(203.461510251184,98.4897376070391,334.091286083065));
#27063=CARTESIAN_POINT('Ctrl Pts',(205.525249403466,98.4272376070391,334.265362482058));
#27064=CARTESIAN_POINT('Ctrl Pts',(206.861442750472,98.3647376070391,335.847737033408));
#27065=CARTESIAN_POINT('Ctrl Pts',(208.197636097478,98.3022376070391,337.430111584758));
#27066=CARTESIAN_POINT('Ctrl Pts',(208.023559698486,98.2397376070391,339.49385073704));
#27067=CARTESIAN_POINT('Ctrl Pts',(207.849483299494,98.1772376070391,341.557589889321));
#27068=CARTESIAN_POINT('Ctrl Pts',(206.267108748143,98.1147376070391,342.893783236327));
#27069=CARTESIAN_POINT('Ctrl Pts',(204.684734196793,98.0522376070391,344.229976583334));
#27070=CARTESIAN_POINT('Ctrl Pts',(202.620995044512,97.989737607039,344.055900184342));
#27071=CARTESIAN_POINT('Ctrl Pts',(200.55725589223,97.9272376070391,343.881823785349));
#27072=CARTESIAN_POINT('Ctrl Pts',(199.221062545224,97.8647376070391,342.299449233999));
#27073=CARTESIAN_POINT('Ctrl Pts',(197.884869198218,97.8022376070391,340.717074682649));
#27074=CARTESIAN_POINT('Ctrl Pts',(198.05894559721,97.739737607039,338.653335530367));
#27075=CARTESIAN_POINT('Ctrl Pts',(198.233021996202,97.6772376070391,336.589596378086));
#27076=CARTESIAN_POINT('Ctrl Pts',(199.815396547552,97.6147376070391,335.253403031079));
#27077=CARTESIAN_POINT('Ctrl Pts',(201.397771098903,97.5522376070391,333.917209684073));
#27078=CARTESIAN_POINT('Ctrl Pts',(203.461510251184,97.489737607039,334.091286083065));
#27079=CARTESIAN_POINT('Ctrl Pts',(205.525249403466,97.4272376070391,334.265362482058));
#27080=CARTESIAN_POINT('Ctrl Pts',(206.861442750472,97.3647376070391,335.847737033408));
#27081=CARTESIAN_POINT('Ctrl Pts',(208.197636097478,97.3022376070391,337.430111584758));
#27082=CARTESIAN_POINT('Ctrl Pts',(208.023559698486,97.2397376070391,339.49385073704));
#27083=CARTESIAN_POINT('Ctrl Pts',(207.849483299494,97.1772376070391,341.557589889321));
#27084=CARTESIAN_POINT('Ctrl Pts',(206.267108748143,97.1147376070391,342.893783236327));
#27085=CARTESIAN_POINT('Ctrl Pts',(204.684734196793,97.0522376070391,344.229976583334));
#27086=CARTESIAN_POINT('Ctrl Pts',(202.620995044512,96.9897376070391,344.055900184342));
#27087=CARTESIAN_POINT('Ctrl Pts',(200.55725589223,96.9272376070391,343.881823785349));
#27088=CARTESIAN_POINT('Ctrl Pts',(199.221062545224,96.8647376070391,342.299449233999));
#27089=CARTESIAN_POINT('Ctrl Pts',(197.884869198218,96.8022376070391,340.717074682649));
#27090=CARTESIAN_POINT('Ctrl Pts',(198.05894559721,96.739737607039,338.653335530367));
#27091=CARTESIAN_POINT('Ctrl Pts',(198.233021996202,96.6772376070391,336.589596378086));
#27092=CARTESIAN_POINT('Ctrl Pts',(199.815396547552,96.6147376070391,335.253403031079));
#27093=CARTESIAN_POINT('Ctrl Pts',(201.397771098903,96.552237607039,333.917209684073));
#27094=CARTESIAN_POINT('Ctrl Pts',(203.461510251184,96.4897376070391,334.091286083065));
#27095=CARTESIAN_POINT('Ctrl Pts',(205.525249403466,96.4272376070391,334.265362482058));
#27096=CARTESIAN_POINT('Ctrl Pts',(206.861442750472,96.3647376070391,335.847737033408));
#27097=CARTESIAN_POINT('Ctrl Pts',(208.197636097478,96.3022376070391,337.430111584758));
#27098=CARTESIAN_POINT('Ctrl Pts',(208.023559698486,96.2397376070391,339.49385073704));
#27099=CARTESIAN_POINT('Ctrl Pts',(207.849483299494,96.1772376070391,341.557589889321));
#27100=CARTESIAN_POINT('Ctrl Pts',(206.267108748143,96.1147376070391,342.893783236327));
#27101=CARTESIAN_POINT('Ctrl Pts',(204.684734196793,96.0522376070391,344.229976583334));
#27102=CARTESIAN_POINT('Ctrl Pts',(202.620995044512,95.9897376070391,344.055900184342));
#27103=CARTESIAN_POINT('Ctrl Pts',(200.55725589223,95.9272376070391,343.881823785349));
#27104=CARTESIAN_POINT('Ctrl Pts',(199.221062545224,95.8647376070391,342.299449233999));
#27105=CARTESIAN_POINT('Ctrl Pts',(197.884869198218,95.8022376070391,340.717074682649));
#27106=CARTESIAN_POINT('Ctrl Pts',(198.05894559721,95.7397376070391,338.653335530367));
#27107=CARTESIAN_POINT('Ctrl Pts',(198.233021996202,95.6772376070391,336.589596378086));
#27108=CARTESIAN_POINT('Ctrl Pts',(199.815396547552,95.6147376070391,335.253403031079));
#27109=CARTESIAN_POINT('Ctrl Pts',(201.397771098903,95.5522376070391,333.917209684073));
#27110=CARTESIAN_POINT('Ctrl Pts',(203.461510251184,95.4897376070391,334.091286083065));
#27111=CARTESIAN_POINT('Ctrl Pts',(205.525249403466,95.4272376070391,334.265362482058));
#27112=CARTESIAN_POINT('Ctrl Pts',(206.861442750472,95.3647376070391,335.847737033408));
#27113=CARTESIAN_POINT('Ctrl Pts',(208.197636097478,95.3022376070391,337.430111584758));
#27114=CARTESIAN_POINT('Ctrl Pts',(208.023559698486,95.2397376070391,339.49385073704));
#27115=CARTESIAN_POINT('Ctrl Pts',(207.849483299494,95.1772376070391,341.557589889321));
#27116=CARTESIAN_POINT('Ctrl Pts',(206.267108748143,95.1147376070391,342.893783236327));
#27117=CARTESIAN_POINT('Ctrl Pts',(204.684734196793,95.0522376070391,344.229976583334));
#27118=CARTESIAN_POINT('Ctrl Pts',(202.620995044512,94.9897376070391,344.055900184342));
#27119=CARTESIAN_POINT('Ctrl Pts',(200.55725589223,94.9272376070391,343.881823785349));
#27120=CARTESIAN_POINT('Ctrl Pts',(199.221062545224,94.8647376070391,342.299449233999));
#27121=CARTESIAN_POINT('Ctrl Pts',(197.884869198218,94.8022376070391,340.717074682649));
#27122=CARTESIAN_POINT('Ctrl Pts',(198.05894559721,94.7397376070391,338.653335530367));
#27123=CARTESIAN_POINT('Ctrl Pts',(198.233021996202,94.6772376070391,336.589596378086));
#27124=CARTESIAN_POINT('Ctrl Pts',(199.815396547552,94.6147376070391,335.253403031079));
#27125=CARTESIAN_POINT('Ctrl Pts',(201.397771098903,94.5522376070391,333.917209684073));
#27126=CARTESIAN_POINT('Ctrl Pts',(203.461510251184,94.4897376070391,334.091286083065));
#27127=CARTESIAN_POINT('Ctrl Pts',(205.525249403466,94.4272376070391,334.265362482058));
#27128=CARTESIAN_POINT('Ctrl Pts',(206.861442750472,94.3647376070391,335.847737033408));
#27129=CARTESIAN_POINT('Ctrl Pts',(208.197636097478,94.3022376070391,337.430111584758));
#27130=CARTESIAN_POINT('Ctrl Pts',(208.023559698486,94.2397376070391,339.49385073704));
#27131=CARTESIAN_POINT('Ctrl Pts',(207.849483299494,94.1772376070391,341.557589889321));
#27132=CARTESIAN_POINT('Ctrl Pts',(206.267108748143,94.1147376070391,342.893783236327));
#27133=CARTESIAN_POINT('Ctrl Pts',(204.684734196793,94.0522376070391,344.229976583334));
#27134=CARTESIAN_POINT('Ctrl Pts',(202.620995044512,93.9897376070391,344.055900184342));
#27135=CARTESIAN_POINT('Ctrl Pts',(200.55725589223,93.9272376070391,343.881823785349));
#27136=CARTESIAN_POINT('Ctrl Pts',(199.221062545224,93.8647376070391,342.299449233999));
#27137=CARTESIAN_POINT('Ctrl Pts',(197.884869198218,93.8022376070391,340.717074682649));
#27138=CARTESIAN_POINT('Ctrl Pts',(198.05894559721,93.7397376070391,338.653335530367));
#27139=CARTESIAN_POINT('Ctrl Pts',(198.233021996202,93.6772376070391,336.589596378086));
#27140=CARTESIAN_POINT('Ctrl Pts',(199.815396547552,93.6147376070391,335.253403031079));
#27141=CARTESIAN_POINT('Ctrl Pts',(201.397771098903,93.5522376070391,333.917209684073));
#27142=CARTESIAN_POINT('Ctrl Pts',(203.461510251184,93.4897376070391,334.091286083065));
#27143=CARTESIAN_POINT('Ctrl Pts',(205.525249403466,93.4272376070391,334.265362482058));
#27144=CARTESIAN_POINT('Ctrl Pts',(206.861442750472,93.3647376070391,335.847737033408));
#27145=CARTESIAN_POINT('Ctrl Pts',(208.197636097478,93.3022376070391,337.430111584758));
#27146=CARTESIAN_POINT('Ctrl Pts',(208.023559698486,93.2397376070391,339.49385073704));
#27147=CARTESIAN_POINT('Ctrl Pts',(207.849483299494,93.1772376070391,341.557589889321));
#27148=CARTESIAN_POINT('Ctrl Pts',(206.267108748143,93.1147376070391,342.893783236327));
#27149=CARTESIAN_POINT('Ctrl Pts',(204.684734196793,93.0522376070391,344.229976583334));
#27150=CARTESIAN_POINT('Ctrl Pts',(202.620995044512,92.9897376070391,344.055900184342));
#27151=CARTESIAN_POINT('Ctrl Pts',(200.55725589223,92.9272376070391,343.881823785349));
#27152=CARTESIAN_POINT('Ctrl Pts',(199.221062545224,92.8647376070391,342.299449233999));
#27153=CARTESIAN_POINT('Ctrl Pts',(197.884869198218,92.8022376070391,340.717074682649));
#27154=CARTESIAN_POINT('Ctrl Pts',(198.05894559721,92.7397376070391,338.653335530367));
#27155=CARTESIAN_POINT('Ctrl Pts',(198.233021996202,92.6772376070391,336.589596378086));
#27156=CARTESIAN_POINT('Ctrl Pts',(199.815396547552,92.6147376070391,335.253403031079));
#27157=CARTESIAN_POINT('Ctrl Pts',(201.397771098903,92.5522376070391,333.917209684073));
#27158=CARTESIAN_POINT('Ctrl Pts',(203.461510251184,92.4897376070391,334.091286083065));
#27159=CARTESIAN_POINT('Ctrl Pts',(205.525249403466,92.4272376070391,334.265362482058));
#27160=CARTESIAN_POINT('Ctrl Pts',(206.861442750472,92.3647376070391,335.847737033408));
#27161=CARTESIAN_POINT('Ctrl Pts',(208.197636097478,92.3022376070391,337.430111584758));
#27162=CARTESIAN_POINT('Ctrl Pts',(208.023559698486,92.2397376070391,339.49385073704));
#27163=CARTESIAN_POINT('Ctrl Pts',(207.849483299494,92.1772376070391,341.557589889321));
#27164=CARTESIAN_POINT('Ctrl Pts',(206.267108748143,92.1147376070391,342.893783236327));
#27165=CARTESIAN_POINT('Ctrl Pts',(204.684734196793,92.0522376070391,344.229976583334));
#27166=CARTESIAN_POINT('Ctrl Pts',(202.620995044512,91.9897376070391,344.055900184342));
#27167=CARTESIAN_POINT('Ctrl Pts',(200.55725589223,91.9272376070391,343.881823785349));
#27168=CARTESIAN_POINT('Ctrl Pts',(199.221062545224,91.8647376070391,342.299449233999));
#27169=CARTESIAN_POINT('Ctrl Pts',(197.884869198218,91.8022376070391,340.717074682649));
#27170=CARTESIAN_POINT('Ctrl Pts',(198.05894559721,91.7397376070391,338.653335530367));
#27171=CARTESIAN_POINT('Ctrl Pts',(198.233021996202,91.6772376070391,336.589596378086));
#27172=CARTESIAN_POINT('Ctrl Pts',(199.815396547552,91.6147376070391,335.253403031079));
#27173=CARTESIAN_POINT('Ctrl Pts',(201.397771098903,91.5522376070391,333.917209684073));
#27174=CARTESIAN_POINT('Ctrl Pts',(203.461510251184,91.4897376070391,334.091286083065));
#27175=CARTESIAN_POINT('Ctrl Pts',(205.525249403466,91.4272376070391,334.265362482058));
#27176=CARTESIAN_POINT('Ctrl Pts',(206.861442750472,91.3647376070391,335.847737033408));
#27177=CARTESIAN_POINT('Ctrl Pts',(208.197636097478,91.3022376070391,337.430111584758));
#27178=CARTESIAN_POINT('Ctrl Pts',(208.023559698486,91.2397376070391,339.49385073704));
#27179=CARTESIAN_POINT('Ctrl Pts',(207.849483299494,91.1772376070391,341.557589889321));
#27180=CARTESIAN_POINT('Ctrl Pts',(206.267108748143,91.1147376070391,342.893783236327));
#27181=CARTESIAN_POINT('Ctrl Pts',(204.684734196793,91.0522376070391,344.229976583334));
#27182=CARTESIAN_POINT('Ctrl Pts',(202.620995044512,90.9897376070391,344.055900184342));
#27183=CARTESIAN_POINT('Ctrl Pts',(200.55725589223,90.9272376070391,343.881823785349));
#27184=CARTESIAN_POINT('Ctrl Pts',(199.221062545224,90.8647376070391,342.299449233999));
#27185=CARTESIAN_POINT('Ctrl Pts',(197.884869198218,90.8022376070391,340.717074682649));
#27186=CARTESIAN_POINT('Ctrl Pts',(198.05894559721,90.7397376070391,338.653335530367));
#27187=CARTESIAN_POINT('Ctrl Pts',(198.233021996202,90.6772376070391,336.589596378086));
#27188=CARTESIAN_POINT('Ctrl Pts',(199.815396547552,90.6147376070391,335.253403031079));
#27189=CARTESIAN_POINT('Ctrl Pts',(201.397771098903,90.5522376070391,333.917209684073));
#27190=CARTESIAN_POINT('Ctrl Pts',(203.461510251184,90.4897376070391,334.091286083065));
#27191=CARTESIAN_POINT('Ctrl Pts',(205.525249403466,90.4272376070391,334.265362482058));
#27192=CARTESIAN_POINT('Ctrl Pts',(206.861442750472,90.3647376070391,335.847737033408));
#27193=CARTESIAN_POINT('Ctrl Pts',(208.197636097478,90.3022376070391,337.430111584758));
#27194=CARTESIAN_POINT('Ctrl Pts',(208.023559698486,90.2397376070391,339.49385073704));
#27195=CARTESIAN_POINT('Ctrl Pts',(207.849483299494,90.1772376070391,341.557589889321));
#27196=CARTESIAN_POINT('Ctrl Pts',(206.267108748143,90.1147376070391,342.893783236327));
#27197=CARTESIAN_POINT('Ctrl Pts',(204.684734196793,90.0522376070391,344.229976583334));
#27198=CARTESIAN_POINT('Ctrl Pts',(202.620995044512,89.9897376070391,344.055900184342));
#27199=CARTESIAN_POINT('Ctrl Pts',(200.55725589223,89.9272376070391,343.881823785349));
#27200=CARTESIAN_POINT('Ctrl Pts',(199.221062545224,89.8647376070391,342.299449233999));
#27201=CARTESIAN_POINT('Ctrl Pts',(197.884869198218,89.8022376070391,340.717074682649));
#27202=CARTESIAN_POINT('Ctrl Pts',(198.05894559721,89.7397376070391,338.653335530367));
#27203=CARTESIAN_POINT('Ctrl Pts',(197.519595040153,99.4272376084047,338.607841310488));
#27204=CARTESIAN_POINT('Ctrl Pts',(197.712515762029,99.3647376084047,336.320695842601));
#27205=CARTESIAN_POINT('Ctrl Pts',(199.466187382602,99.3022376084047,334.839855323367));
#27206=CARTESIAN_POINT('Ctrl Pts',(201.219859003176,99.2397376084047,333.359014804133));
#27207=CARTESIAN_POINT('Ctrl Pts',(203.507004471063,99.1772376084047,333.551935526009));
#27208=CARTESIAN_POINT('Ctrl Pts',(205.794149938951,99.1147376084047,333.744856247885));
#27209=CARTESIAN_POINT('Ctrl Pts',(207.274990458185,99.0522376084047,335.498527868458));
#27210=CARTESIAN_POINT('Ctrl Pts',(208.755830977418,98.9897376084047,337.252199489031));
#27211=CARTESIAN_POINT('Ctrl Pts',(208.562910255543,98.9272376084047,339.539344956919));
#27212=CARTESIAN_POINT('Ctrl Pts',(208.369989533667,98.8647376084047,341.826490424806));
#27213=CARTESIAN_POINT('Ctrl Pts',(206.616317913094,98.8022376084047,343.30733094404));
#27214=CARTESIAN_POINT('Ctrl Pts',(204.86264629252,98.7397376084047,344.788171463274));
#27215=CARTESIAN_POINT('Ctrl Pts',(202.575500824633,98.6772376084047,344.595250741398));
#27216=CARTESIAN_POINT('Ctrl Pts',(200.288355356745,98.6147376084047,344.402330019522));
#27217=CARTESIAN_POINT('Ctrl Pts',(198.807514837511,98.5522376084047,342.648658398949));
#27218=CARTESIAN_POINT('Ctrl Pts',(197.326674318278,98.4897376084047,340.894986778376));
#27219=CARTESIAN_POINT('Ctrl Pts',(197.519595040153,98.4272376084047,338.607841310488));
#27220=CARTESIAN_POINT('Ctrl Pts',(197.712515762029,98.3647376084047,336.320695842601));
#27221=CARTESIAN_POINT('Ctrl Pts',(199.466187382602,98.3022376084047,334.839855323367));
#27222=CARTESIAN_POINT('Ctrl Pts',(201.219859003176,98.2397376084047,333.359014804133));
#27223=CARTESIAN_POINT('Ctrl Pts',(203.507004471063,98.1772376084047,333.551935526009));
#27224=CARTESIAN_POINT('Ctrl Pts',(205.794149938951,98.1147376084047,333.744856247885));
#27225=CARTESIAN_POINT('Ctrl Pts',(207.274990458185,98.0522376084047,335.498527868458));
#27226=CARTESIAN_POINT('Ctrl Pts',(208.755830977418,97.9897376084047,337.252199489031));
#27227=CARTESIAN_POINT('Ctrl Pts',(208.562910255543,97.9272376084047,339.539344956919));
#27228=CARTESIAN_POINT('Ctrl Pts',(208.369989533667,97.8647376084047,341.826490424806));
#27229=CARTESIAN_POINT('Ctrl Pts',(206.616317913094,97.8022376084047,343.30733094404));
#27230=CARTESIAN_POINT('Ctrl Pts',(204.86264629252,97.7397376084047,344.788171463274));
#27231=CARTESIAN_POINT('Ctrl Pts',(202.575500824633,97.6772376084047,344.595250741398));
#27232=CARTESIAN_POINT('Ctrl Pts',(200.288355356745,97.6147376084047,344.402330019522));
#27233=CARTESIAN_POINT('Ctrl Pts',(198.807514837511,97.5522376084047,342.648658398949));
#27234=CARTESIAN_POINT('Ctrl Pts',(197.326674318278,97.4897376084047,340.894986778376));
#27235=CARTESIAN_POINT('Ctrl Pts',(197.519595040153,97.4272376084047,338.607841310488));
#27236=CARTESIAN_POINT('Ctrl Pts',(197.712515762029,97.3647376084047,336.320695842601));
#27237=CARTESIAN_POINT('Ctrl Pts',(199.466187382602,97.3022376084047,334.839855323367));
#27238=CARTESIAN_POINT('Ctrl Pts',(201.219859003176,97.2397376084047,333.359014804133));
#27239=CARTESIAN_POINT('Ctrl Pts',(203.507004471063,97.1772376084047,333.551935526009));
#27240=CARTESIAN_POINT('Ctrl Pts',(205.794149938951,97.1147376084047,333.744856247885));
#27241=CARTESIAN_POINT('Ctrl Pts',(207.274990458185,97.0522376084047,335.498527868458));
#27242=CARTESIAN_POINT('Ctrl Pts',(208.755830977418,96.9897376084047,337.252199489031));
#27243=CARTESIAN_POINT('Ctrl Pts',(208.562910255543,96.9272376084047,339.539344956919));
#27244=CARTESIAN_POINT('Ctrl Pts',(208.369989533667,96.8647376084047,341.826490424806));
#27245=CARTESIAN_POINT('Ctrl Pts',(206.616317913094,96.8022376084046,343.30733094404));
#27246=CARTESIAN_POINT('Ctrl Pts',(204.86264629252,96.7397376084047,344.788171463274));
#27247=CARTESIAN_POINT('Ctrl Pts',(202.575500824633,96.6772376084047,344.595250741398));
#27248=CARTESIAN_POINT('Ctrl Pts',(200.288355356745,96.6147376084047,344.402330019522));
#27249=CARTESIAN_POINT('Ctrl Pts',(198.807514837511,96.5522376084046,342.648658398949));
#27250=CARTESIAN_POINT('Ctrl Pts',(197.326674318278,96.4897376084047,340.894986778376));
#27251=CARTESIAN_POINT('Ctrl Pts',(197.519595040153,96.4272376084047,338.607841310488));
#27252=CARTESIAN_POINT('Ctrl Pts',(197.712515762029,96.3647376084047,336.320695842601));
#27253=CARTESIAN_POINT('Ctrl Pts',(199.466187382602,96.3022376084047,334.839855323367));
#27254=CARTESIAN_POINT('Ctrl Pts',(201.219859003176,96.2397376084047,333.359014804133));
#27255=CARTESIAN_POINT('Ctrl Pts',(203.507004471063,96.1772376084047,333.551935526009));
#27256=CARTESIAN_POINT('Ctrl Pts',(205.794149938951,96.1147376084047,333.744856247885));
#27257=CARTESIAN_POINT('Ctrl Pts',(207.274990458185,96.0522376084047,335.498527868458));
#27258=CARTESIAN_POINT('Ctrl Pts',(208.755830977418,95.9897376084047,337.252199489031));
#27259=CARTESIAN_POINT('Ctrl Pts',(208.562910255543,95.9272376084047,339.539344956919));
#27260=CARTESIAN_POINT('Ctrl Pts',(208.369989533667,95.8647376084047,341.826490424806));
#27261=CARTESIAN_POINT('Ctrl Pts',(206.616317913094,95.8022376084047,343.30733094404));
#27262=CARTESIAN_POINT('Ctrl Pts',(204.86264629252,95.7397376084047,344.788171463274));
#27263=CARTESIAN_POINT('Ctrl Pts',(202.575500824633,95.6772376084046,344.595250741398));
#27264=CARTESIAN_POINT('Ctrl Pts',(200.288355356745,95.6147376084047,344.402330019522));
#27265=CARTESIAN_POINT('Ctrl Pts',(198.807514837511,95.5522376084046,342.648658398949));
#27266=CARTESIAN_POINT('Ctrl Pts',(197.326674318278,95.4897376084047,340.894986778376));
#27267=CARTESIAN_POINT('Ctrl Pts',(197.519595040153,95.4272376084047,338.607841310488));
#27268=CARTESIAN_POINT('Ctrl Pts',(197.712515762029,95.3647376084047,336.320695842601));
#27269=CARTESIAN_POINT('Ctrl Pts',(199.466187382602,95.3022376084047,334.839855323367));
#27270=CARTESIAN_POINT('Ctrl Pts',(201.219859003176,95.2397376084047,333.359014804133));
#27271=CARTESIAN_POINT('Ctrl Pts',(203.507004471063,95.1772376084047,333.551935526009));
#27272=CARTESIAN_POINT('Ctrl Pts',(205.794149938951,95.1147376084047,333.744856247885));
#27273=CARTESIAN_POINT('Ctrl Pts',(207.274990458185,95.0522376084046,335.498527868458));
#27274=CARTESIAN_POINT('Ctrl Pts',(208.755830977418,94.9897376084047,337.252199489031));
#27275=CARTESIAN_POINT('Ctrl Pts',(208.562910255543,94.9272376084047,339.539344956919));
#27276=CARTESIAN_POINT('Ctrl Pts',(208.369989533667,94.8647376084047,341.826490424806));
#27277=CARTESIAN_POINT('Ctrl Pts',(206.616317913094,94.8022376084047,343.30733094404));
#27278=CARTESIAN_POINT('Ctrl Pts',(204.86264629252,94.7397376084047,344.788171463274));
#27279=CARTESIAN_POINT('Ctrl Pts',(202.575500824633,94.6772376084047,344.595250741398));
#27280=CARTESIAN_POINT('Ctrl Pts',(200.288355356745,94.6147376084047,344.402330019522));
#27281=CARTESIAN_POINT('Ctrl Pts',(198.807514837511,94.5522376084047,342.648658398949));
#27282=CARTESIAN_POINT('Ctrl Pts',(197.326674318278,94.4897376084047,340.894986778376));
#27283=CARTESIAN_POINT('Ctrl Pts',(197.519595040153,94.4272376084047,338.607841310488));
#27284=CARTESIAN_POINT('Ctrl Pts',(197.712515762029,94.3647376084047,336.320695842601));
#27285=CARTESIAN_POINT('Ctrl Pts',(199.466187382602,94.3022376084047,334.839855323367));
#27286=CARTESIAN_POINT('Ctrl Pts',(201.219859003176,94.2397376084047,333.359014804133));
#27287=CARTESIAN_POINT('Ctrl Pts',(203.507004471063,94.1772376084047,333.551935526009));
#27288=CARTESIAN_POINT('Ctrl Pts',(205.794149938951,94.1147376084047,333.744856247885));
#27289=CARTESIAN_POINT('Ctrl Pts',(207.274990458185,94.0522376084047,335.498527868458));
#27290=CARTESIAN_POINT('Ctrl Pts',(208.755830977418,93.9897376084047,337.252199489031));
#27291=CARTESIAN_POINT('Ctrl Pts',(208.562910255543,93.9272376084047,339.539344956919));
#27292=CARTESIAN_POINT('Ctrl Pts',(208.369989533667,93.8647376084047,341.826490424806));
#27293=CARTESIAN_POINT('Ctrl Pts',(206.616317913094,93.8022376084047,343.30733094404));
#27294=CARTESIAN_POINT('Ctrl Pts',(204.86264629252,93.7397376084047,344.788171463274));
#27295=CARTESIAN_POINT('Ctrl Pts',(202.575500824633,93.6772376084047,344.595250741398));
#27296=CARTESIAN_POINT('Ctrl Pts',(200.288355356745,93.6147376084047,344.402330019522));
#27297=CARTESIAN_POINT('Ctrl Pts',(198.807514837511,93.5522376084047,342.648658398949));
#27298=CARTESIAN_POINT('Ctrl Pts',(197.326674318278,93.4897376084047,340.894986778376));
#27299=CARTESIAN_POINT('Ctrl Pts',(197.519595040153,93.4272376084047,338.607841310488));
#27300=CARTESIAN_POINT('Ctrl Pts',(197.712515762029,93.3647376084047,336.320695842601));
#27301=CARTESIAN_POINT('Ctrl Pts',(199.466187382602,93.3022376084047,334.839855323367));
#27302=CARTESIAN_POINT('Ctrl Pts',(201.219859003176,93.2397376084047,333.359014804133));
#27303=CARTESIAN_POINT('Ctrl Pts',(203.507004471063,93.1772376084047,333.551935526009));
#27304=CARTESIAN_POINT('Ctrl Pts',(205.794149938951,93.1147376084047,333.744856247885));
#27305=CARTESIAN_POINT('Ctrl Pts',(207.274990458185,93.0522376084047,335.498527868458));
#27306=CARTESIAN_POINT('Ctrl Pts',(208.755830977418,92.9897376084047,337.252199489031));
#27307=CARTESIAN_POINT('Ctrl Pts',(208.562910255543,92.9272376084047,339.539344956919));
#27308=CARTESIAN_POINT('Ctrl Pts',(208.369989533667,92.8647376084047,341.826490424806));
#27309=CARTESIAN_POINT('Ctrl Pts',(206.616317913094,92.8022376084047,343.30733094404));
#27310=CARTESIAN_POINT('Ctrl Pts',(204.86264629252,92.7397376084047,344.788171463274));
#27311=CARTESIAN_POINT('Ctrl Pts',(202.575500824633,92.6772376084047,344.595250741398));
#27312=CARTESIAN_POINT('Ctrl Pts',(200.288355356745,92.6147376084047,344.402330019522));
#27313=CARTESIAN_POINT('Ctrl Pts',(198.807514837511,92.5522376084047,342.648658398949));
#27314=CARTESIAN_POINT('Ctrl Pts',(197.326674318278,92.4897376084047,340.894986778376));
#27315=CARTESIAN_POINT('Ctrl Pts',(197.519595040153,92.4272376084047,338.607841310488));
#27316=CARTESIAN_POINT('Ctrl Pts',(197.712515762029,92.3647376084047,336.320695842601));
#27317=CARTESIAN_POINT('Ctrl Pts',(199.466187382602,92.3022376084047,334.839855323367));
#27318=CARTESIAN_POINT('Ctrl Pts',(201.219859003176,92.2397376084047,333.359014804133));
#27319=CARTESIAN_POINT('Ctrl Pts',(203.507004471063,92.1772376084047,333.551935526009));
#27320=CARTESIAN_POINT('Ctrl Pts',(205.794149938951,92.1147376084047,333.744856247885));
#27321=CARTESIAN_POINT('Ctrl Pts',(207.274990458185,92.0522376084047,335.498527868458));
#27322=CARTESIAN_POINT('Ctrl Pts',(208.755830977418,91.9897376084047,337.252199489031));
#27323=CARTESIAN_POINT('Ctrl Pts',(208.562910255543,91.9272376084047,339.539344956919));
#27324=CARTESIAN_POINT('Ctrl Pts',(208.369989533667,91.8647376084047,341.826490424806));
#27325=CARTESIAN_POINT('Ctrl Pts',(206.616317913094,91.8022376084047,343.30733094404));
#27326=CARTESIAN_POINT('Ctrl Pts',(204.86264629252,91.7397376084047,344.788171463274));
#27327=CARTESIAN_POINT('Ctrl Pts',(202.575500824633,91.6772376084047,344.595250741398));
#27328=CARTESIAN_POINT('Ctrl Pts',(200.288355356745,91.6147376084047,344.402330019522));
#27329=CARTESIAN_POINT('Ctrl Pts',(198.807514837511,91.5522376084047,342.648658398949));
#27330=CARTESIAN_POINT('Ctrl Pts',(197.326674318278,91.4897376084047,340.894986778376));
#27331=CARTESIAN_POINT('Ctrl Pts',(197.519595040153,91.4272376084047,338.607841310488));
#27332=CARTESIAN_POINT('Ctrl Pts',(197.712515762029,91.3647376084047,336.320695842601));
#27333=CARTESIAN_POINT('Ctrl Pts',(199.466187382602,91.3022376084047,334.839855323367));
#27334=CARTESIAN_POINT('Ctrl Pts',(201.219859003176,91.2397376084047,333.359014804133));
#27335=CARTESIAN_POINT('Ctrl Pts',(203.507004471063,91.1772376084047,333.551935526009));
#27336=CARTESIAN_POINT('Ctrl Pts',(205.794149938951,91.1147376084047,333.744856247885));
#27337=CARTESIAN_POINT('Ctrl Pts',(207.274990458185,91.0522376084047,335.498527868458));
#27338=CARTESIAN_POINT('Ctrl Pts',(208.755830977418,90.9897376084047,337.252199489031));
#27339=CARTESIAN_POINT('Ctrl Pts',(208.562910255543,90.9272376084047,339.539344956919));
#27340=CARTESIAN_POINT('Ctrl Pts',(208.369989533667,90.8647376084047,341.826490424806));
#27341=CARTESIAN_POINT('Ctrl Pts',(206.616317913094,90.8022376084047,343.30733094404));
#27342=CARTESIAN_POINT('Ctrl Pts',(204.86264629252,90.7397376084047,344.788171463274));
#27343=CARTESIAN_POINT('Ctrl Pts',(202.575500824633,90.6772376084047,344.595250741398));
#27344=CARTESIAN_POINT('Ctrl Pts',(200.288355356745,90.6147376084047,344.402330019522));
#27345=CARTESIAN_POINT('Ctrl Pts',(198.807514837511,90.5522376084047,342.648658398949));
#27346=CARTESIAN_POINT('Ctrl Pts',(197.326674318278,90.4897376084047,340.894986778376));
#27347=CARTESIAN_POINT('Ctrl Pts',(197.519595040153,90.4272376084047,338.607841310488));
#27348=CARTESIAN_POINT('Ctrl Pts',(197.712515762029,90.3647376084047,336.320695842601));
#27349=CARTESIAN_POINT('Ctrl Pts',(199.466187382602,90.3022376084047,334.839855323367));
#27350=CARTESIAN_POINT('Ctrl Pts',(201.219859003176,90.2397376084047,333.359014804133));
#27351=CARTESIAN_POINT('Ctrl Pts',(203.507004471063,90.1772376084047,333.551935526009));
#27352=CARTESIAN_POINT('Ctrl Pts',(205.794149938951,90.1147376084047,333.744856247885));
#27353=CARTESIAN_POINT('Ctrl Pts',(207.274990458185,90.0522376084047,335.498527868458));
#27354=CARTESIAN_POINT('Ctrl Pts',(208.755830977418,89.9897376084047,337.252199489031));
#27355=CARTESIAN_POINT('Ctrl Pts',(208.562910255543,89.9272376084047,339.539344956919));
#27356=CARTESIAN_POINT('Ctrl Pts',(208.369989533667,89.8647376084047,341.826490424806));
#27357=CARTESIAN_POINT('Ctrl Pts',(206.616317913094,89.8022376084047,343.30733094404));
#27358=CARTESIAN_POINT('Ctrl Pts',(204.86264629252,89.7397376084047,344.788171463274));
#27359=CARTESIAN_POINT('Ctrl Pts',(202.575500824633,89.6772376084047,344.595250741398));
#27360=CARTESIAN_POINT('Ctrl Pts',(200.288355356745,89.6147376084047,344.402330019522));
#27361=CARTESIAN_POINT('Ctrl Pts',(198.807514837511,89.5522376084047,342.648658398949));
#27362=CARTESIAN_POINT('Ctrl Pts',(197.326674318278,89.4897376084047,340.894986778376));
#27363=CARTESIAN_POINT('Ctrl Pts',(197.519595040153,89.4272376084047,338.607841310488));
#27364=CARTESIAN_POINT('Ctrl Pts',(197.519595040153,99.3022376084047,338.607841310488));
#27365=CARTESIAN_POINT('Ctrl Pts',(197.712515762029,99.2397376084047,336.320695842601));
#27366=CARTESIAN_POINT('Ctrl Pts',(199.466187382602,99.1772376084047,334.839855323367));
#27367=CARTESIAN_POINT('Ctrl Pts',(201.219859003176,99.1147376084047,333.359014804133));
#27368=CARTESIAN_POINT('Ctrl Pts',(203.507004471063,99.0522376084047,333.551935526009));
#27369=CARTESIAN_POINT('Ctrl Pts',(205.794149938951,98.9897376084047,333.744856247885));
#27370=CARTESIAN_POINT('Ctrl Pts',(207.274990458185,98.9272376084047,335.498527868458));
#27371=CARTESIAN_POINT('Ctrl Pts',(208.755830977418,98.8647376084047,337.252199489031));
#27372=CARTESIAN_POINT('Ctrl Pts',(208.562910255543,98.8022376084047,339.539344956919));
#27373=CARTESIAN_POINT('Ctrl Pts',(208.369989533667,98.7397376084047,341.826490424806));
#27374=CARTESIAN_POINT('Ctrl Pts',(206.616317913094,98.6772376084047,343.30733094404));
#27375=CARTESIAN_POINT('Ctrl Pts',(204.86264629252,98.6147376084047,344.788171463274));
#27376=CARTESIAN_POINT('Ctrl Pts',(202.575500824633,98.5522376084047,344.595250741398));
#27377=CARTESIAN_POINT('Ctrl Pts',(200.288355356745,98.4897376084047,344.402330019522));
#27378=CARTESIAN_POINT('Ctrl Pts',(198.807514837511,98.4272376084047,342.648658398949));
#27379=CARTESIAN_POINT('Ctrl Pts',(197.326674318278,98.3647376084047,340.894986778376));
#27380=CARTESIAN_POINT('Ctrl Pts',(197.519595040153,98.3022376084047,338.607841310488));
#27381=CARTESIAN_POINT('Ctrl Pts',(197.712515762029,98.2397376084047,336.320695842601));
#27382=CARTESIAN_POINT('Ctrl Pts',(199.466187382602,98.1772376084047,334.839855323367));
#27383=CARTESIAN_POINT('Ctrl Pts',(201.219859003176,98.1147376084047,333.359014804133));
#27384=CARTESIAN_POINT('Ctrl Pts',(203.507004471063,98.0522376084047,333.551935526009));
#27385=CARTESIAN_POINT('Ctrl Pts',(205.794149938951,97.9897376084047,333.744856247885));
#27386=CARTESIAN_POINT('Ctrl Pts',(207.274990458185,97.9272376084047,335.498527868458));
#27387=CARTESIAN_POINT('Ctrl Pts',(208.755830977418,97.8647376084047,337.252199489031));
#27388=CARTESIAN_POINT('Ctrl Pts',(208.562910255543,97.8022376084047,339.539344956919));
#27389=CARTESIAN_POINT('Ctrl Pts',(208.369989533667,97.7397376084047,341.826490424806));
#27390=CARTESIAN_POINT('Ctrl Pts',(206.616317913094,97.6772376084047,343.30733094404));
#27391=CARTESIAN_POINT('Ctrl Pts',(204.86264629252,97.6147376084047,344.788171463274));
#27392=CARTESIAN_POINT('Ctrl Pts',(202.575500824633,97.5522376084047,344.595250741398));
#27393=CARTESIAN_POINT('Ctrl Pts',(200.288355356745,97.4897376084047,344.402330019522));
#27394=CARTESIAN_POINT('Ctrl Pts',(198.807514837511,97.4272376084047,342.648658398949));
#27395=CARTESIAN_POINT('Ctrl Pts',(197.326674318278,97.3647376084047,340.894986778376));
#27396=CARTESIAN_POINT('Ctrl Pts',(197.519595040153,97.3022376084047,338.607841310488));
#27397=CARTESIAN_POINT('Ctrl Pts',(197.712515762029,97.2397376084047,336.320695842601));
#27398=CARTESIAN_POINT('Ctrl Pts',(199.466187382602,97.1772376084047,334.839855323367));
#27399=CARTESIAN_POINT('Ctrl Pts',(201.219859003176,97.1147376084047,333.359014804133));
#27400=CARTESIAN_POINT('Ctrl Pts',(203.507004471063,97.0522376084047,333.551935526009));
#27401=CARTESIAN_POINT('Ctrl Pts',(205.794149938951,96.9897376084047,333.744856247885));
#27402=CARTESIAN_POINT('Ctrl Pts',(207.274990458185,96.9272376084047,335.498527868458));
#27403=CARTESIAN_POINT('Ctrl Pts',(208.755830977418,96.8647376084047,337.252199489031));
#27404=CARTESIAN_POINT('Ctrl Pts',(208.562910255543,96.8022376084046,339.539344956919));
#27405=CARTESIAN_POINT('Ctrl Pts',(208.369989533667,96.7397376084047,341.826490424806));
#27406=CARTESIAN_POINT('Ctrl Pts',(206.616317913094,96.6772376084047,343.30733094404));
#27407=CARTESIAN_POINT('Ctrl Pts',(204.86264629252,96.6147376084047,344.788171463274));
#27408=CARTESIAN_POINT('Ctrl Pts',(202.575500824633,96.5522376084046,344.595250741398));
#27409=CARTESIAN_POINT('Ctrl Pts',(200.288355356745,96.4897376084047,344.402330019522));
#27410=CARTESIAN_POINT('Ctrl Pts',(198.807514837511,96.4272376084047,342.648658398949));
#27411=CARTESIAN_POINT('Ctrl Pts',(197.326674318278,96.3647376084047,340.894986778376));
#27412=CARTESIAN_POINT('Ctrl Pts',(197.519595040153,96.3022376084047,338.607841310488));
#27413=CARTESIAN_POINT('Ctrl Pts',(197.712515762029,96.2397376084047,336.320695842601));
#27414=CARTESIAN_POINT('Ctrl Pts',(199.466187382602,96.1772376084047,334.839855323367));
#27415=CARTESIAN_POINT('Ctrl Pts',(201.219859003176,96.1147376084047,333.359014804133));
#27416=CARTESIAN_POINT('Ctrl Pts',(203.507004471063,96.0522376084047,333.551935526009));
#27417=CARTESIAN_POINT('Ctrl Pts',(205.794149938951,95.9897376084047,333.744856247885));
#27418=CARTESIAN_POINT('Ctrl Pts',(207.274990458185,95.9272376084047,335.498527868458));
#27419=CARTESIAN_POINT('Ctrl Pts',(208.755830977418,95.8647376084047,337.252199489031));
#27420=CARTESIAN_POINT('Ctrl Pts',(208.562910255543,95.8022376084047,339.539344956919));
#27421=CARTESIAN_POINT('Ctrl Pts',(208.369989533667,95.7397376084047,341.826490424806));
#27422=CARTESIAN_POINT('Ctrl Pts',(206.616317913094,95.6772376084046,343.30733094404));
#27423=CARTESIAN_POINT('Ctrl Pts',(204.86264629252,95.6147376084047,344.788171463274));
#27424=CARTESIAN_POINT('Ctrl Pts',(202.575500824633,95.5522376084046,344.595250741398));
#27425=CARTESIAN_POINT('Ctrl Pts',(200.288355356745,95.4897376084047,344.402330019522));
#27426=CARTESIAN_POINT('Ctrl Pts',(198.807514837511,95.4272376084047,342.648658398949));
#27427=CARTESIAN_POINT('Ctrl Pts',(197.326674318278,95.3647376084047,340.894986778376));
#27428=CARTESIAN_POINT('Ctrl Pts',(197.519595040153,95.3022376084046,338.607841310488));
#27429=CARTESIAN_POINT('Ctrl Pts',(197.712515762029,95.2397376084047,336.320695842601));
#27430=CARTESIAN_POINT('Ctrl Pts',(199.466187382602,95.1772376084047,334.839855323367));
#27431=CARTESIAN_POINT('Ctrl Pts',(201.219859003176,95.1147376084047,333.359014804133));
#27432=CARTESIAN_POINT('Ctrl Pts',(203.507004471063,95.0522376084047,333.551935526009));
#27433=CARTESIAN_POINT('Ctrl Pts',(205.794149938951,94.9897376084047,333.744856247885));
#27434=CARTESIAN_POINT('Ctrl Pts',(207.274990458185,94.9272376084047,335.498527868458));
#27435=CARTESIAN_POINT('Ctrl Pts',(208.755830977418,94.8647376084047,337.252199489031));
#27436=CARTESIAN_POINT('Ctrl Pts',(208.562910255543,94.8022376084047,339.539344956919));
#27437=CARTESIAN_POINT('Ctrl Pts',(208.369989533667,94.7397376084047,341.826490424806));
#27438=CARTESIAN_POINT('Ctrl Pts',(206.616317913094,94.6772376084047,343.30733094404));
#27439=CARTESIAN_POINT('Ctrl Pts',(204.86264629252,94.6147376084047,344.788171463274));
#27440=CARTESIAN_POINT('Ctrl Pts',(202.575500824633,94.5522376084047,344.595250741398));
#27441=CARTESIAN_POINT('Ctrl Pts',(200.288355356745,94.4897376084047,344.402330019522));
#27442=CARTESIAN_POINT('Ctrl Pts',(198.807514837511,94.4272376084047,342.648658398949));
#27443=CARTESIAN_POINT('Ctrl Pts',(197.326674318278,94.3647376084047,340.894986778376));
#27444=CARTESIAN_POINT('Ctrl Pts',(197.519595040153,94.3022376084047,338.607841310488));
#27445=CARTESIAN_POINT('Ctrl Pts',(197.712515762029,94.2397376084047,336.320695842601));
#27446=CARTESIAN_POINT('Ctrl Pts',(199.466187382602,94.1772376084047,334.839855323367));
#27447=CARTESIAN_POINT('Ctrl Pts',(201.219859003176,94.1147376084047,333.359014804133));
#27448=CARTESIAN_POINT('Ctrl Pts',(203.507004471063,94.0522376084047,333.551935526009));
#27449=CARTESIAN_POINT('Ctrl Pts',(205.794149938951,93.9897376084047,333.744856247885));
#27450=CARTESIAN_POINT('Ctrl Pts',(207.274990458185,93.9272376084047,335.498527868458));
#27451=CARTESIAN_POINT('Ctrl Pts',(208.755830977418,93.8647376084047,337.252199489031));
#27452=CARTESIAN_POINT('Ctrl Pts',(208.562910255543,93.8022376084047,339.539344956919));
#27453=CARTESIAN_POINT('Ctrl Pts',(208.369989533667,93.7397376084047,341.826490424806));
#27454=CARTESIAN_POINT('Ctrl Pts',(206.616317913094,93.6772376084047,343.30733094404));
#27455=CARTESIAN_POINT('Ctrl Pts',(204.86264629252,93.6147376084047,344.788171463274));
#27456=CARTESIAN_POINT('Ctrl Pts',(202.575500824633,93.5522376084047,344.595250741398));
#27457=CARTESIAN_POINT('Ctrl Pts',(200.288355356745,93.4897376084047,344.402330019522));
#27458=CARTESIAN_POINT('Ctrl Pts',(198.807514837511,93.4272376084047,342.648658398949));
#27459=CARTESIAN_POINT('Ctrl Pts',(197.326674318278,93.3647376084047,340.894986778376));
#27460=CARTESIAN_POINT('Ctrl Pts',(197.519595040153,93.3022376084047,338.607841310488));
#27461=CARTESIAN_POINT('Ctrl Pts',(197.712515762029,93.2397376084047,336.320695842601));
#27462=CARTESIAN_POINT('Ctrl Pts',(199.466187382602,93.1772376084047,334.839855323367));
#27463=CARTESIAN_POINT('Ctrl Pts',(201.219859003176,93.1147376084047,333.359014804133));
#27464=CARTESIAN_POINT('Ctrl Pts',(203.507004471063,93.0522376084047,333.551935526009));
#27465=CARTESIAN_POINT('Ctrl Pts',(205.794149938951,92.9897376084047,333.744856247885));
#27466=CARTESIAN_POINT('Ctrl Pts',(207.274990458185,92.9272376084047,335.498527868458));
#27467=CARTESIAN_POINT('Ctrl Pts',(208.755830977418,92.8647376084047,337.252199489031));
#27468=CARTESIAN_POINT('Ctrl Pts',(208.562910255543,92.8022376084047,339.539344956919));
#27469=CARTESIAN_POINT('Ctrl Pts',(208.369989533667,92.7397376084047,341.826490424806));
#27470=CARTESIAN_POINT('Ctrl Pts',(206.616317913094,92.6772376084047,343.30733094404));
#27471=CARTESIAN_POINT('Ctrl Pts',(204.86264629252,92.6147376084047,344.788171463274));
#27472=CARTESIAN_POINT('Ctrl Pts',(202.575500824633,92.5522376084047,344.595250741398));
#27473=CARTESIAN_POINT('Ctrl Pts',(200.288355356745,92.4897376084047,344.402330019522));
#27474=CARTESIAN_POINT('Ctrl Pts',(198.807514837511,92.4272376084047,342.648658398949));
#27475=CARTESIAN_POINT('Ctrl Pts',(197.326674318278,92.3647376084047,340.894986778376));
#27476=CARTESIAN_POINT('Ctrl Pts',(197.519595040153,92.3022376084047,338.607841310488));
#27477=CARTESIAN_POINT('Ctrl Pts',(197.712515762029,92.2397376084047,336.320695842601));
#27478=CARTESIAN_POINT('Ctrl Pts',(199.466187382602,92.1772376084047,334.839855323367));
#27479=CARTESIAN_POINT('Ctrl Pts',(201.219859003176,92.1147376084047,333.359014804133));
#27480=CARTESIAN_POINT('Ctrl Pts',(203.507004471063,92.0522376084047,333.551935526009));
#27481=CARTESIAN_POINT('Ctrl Pts',(205.794149938951,91.9897376084047,333.744856247885));
#27482=CARTESIAN_POINT('Ctrl Pts',(207.274990458185,91.9272376084047,335.498527868458));
#27483=CARTESIAN_POINT('Ctrl Pts',(208.755830977418,91.8647376084047,337.252199489031));
#27484=CARTESIAN_POINT('Ctrl Pts',(208.562910255543,91.8022376084047,339.539344956919));
#27485=CARTESIAN_POINT('Ctrl Pts',(208.369989533667,91.7397376084047,341.826490424806));
#27486=CARTESIAN_POINT('Ctrl Pts',(206.616317913094,91.6772376084047,343.30733094404));
#27487=CARTESIAN_POINT('Ctrl Pts',(204.86264629252,91.6147376084047,344.788171463274));
#27488=CARTESIAN_POINT('Ctrl Pts',(202.575500824633,91.5522376084047,344.595250741398));
#27489=CARTESIAN_POINT('Ctrl Pts',(200.288355356745,91.4897376084047,344.402330019522));
#27490=CARTESIAN_POINT('Ctrl Pts',(198.807514837511,91.4272376084047,342.648658398949));
#27491=CARTESIAN_POINT('Ctrl Pts',(197.326674318278,91.3647376084047,340.894986778376));
#27492=CARTESIAN_POINT('Ctrl Pts',(197.519595040153,91.3022376084047,338.607841310488));
#27493=CARTESIAN_POINT('Ctrl Pts',(197.712515762029,91.2397376084047,336.320695842601));
#27494=CARTESIAN_POINT('Ctrl Pts',(199.466187382602,91.1772376084047,334.839855323367));
#27495=CARTESIAN_POINT('Ctrl Pts',(201.219859003176,91.1147376084047,333.359014804133));
#27496=CARTESIAN_POINT('Ctrl Pts',(203.507004471063,91.0522376084047,333.551935526009));
#27497=CARTESIAN_POINT('Ctrl Pts',(205.794149938951,90.9897376084047,333.744856247885));
#27498=CARTESIAN_POINT('Ctrl Pts',(207.274990458185,90.9272376084047,335.498527868458));
#27499=CARTESIAN_POINT('Ctrl Pts',(208.755830977418,90.8647376084047,337.252199489031));
#27500=CARTESIAN_POINT('Ctrl Pts',(208.562910255543,90.8022376084047,339.539344956919));
#27501=CARTESIAN_POINT('Ctrl Pts',(208.369989533667,90.7397376084047,341.826490424806));
#27502=CARTESIAN_POINT('Ctrl Pts',(206.616317913094,90.6772376084047,343.30733094404));
#27503=CARTESIAN_POINT('Ctrl Pts',(204.86264629252,90.6147376084047,344.788171463274));
#27504=CARTESIAN_POINT('Ctrl Pts',(202.575500824633,90.5522376084047,344.595250741398));
#27505=CARTESIAN_POINT('Ctrl Pts',(200.288355356745,90.4897376084047,344.402330019522));
#27506=CARTESIAN_POINT('Ctrl Pts',(198.807514837511,90.4272376084047,342.648658398949));
#27507=CARTESIAN_POINT('Ctrl Pts',(197.326674318278,90.3647376084047,340.894986778376));
#27508=CARTESIAN_POINT('Ctrl Pts',(197.519595040153,90.3022376084047,338.607841310488));
#27509=CARTESIAN_POINT('Ctrl Pts',(197.712515762029,90.2397376084047,336.320695842601));
#27510=CARTESIAN_POINT('Ctrl Pts',(199.466187382602,90.1772376084047,334.839855323367));
#27511=CARTESIAN_POINT('Ctrl Pts',(201.219859003176,90.1147376084047,333.359014804133));
#27512=CARTESIAN_POINT('Ctrl Pts',(203.507004471063,90.0522376084047,333.551935526009));
#27513=CARTESIAN_POINT('Ctrl Pts',(205.794149938951,89.9897376084047,333.744856247885));
#27514=CARTESIAN_POINT('Ctrl Pts',(207.274990458185,89.9272376084047,335.498527868458));
#27515=CARTESIAN_POINT('Ctrl Pts',(208.755830977418,89.8647376084047,337.252199489031));
#27516=CARTESIAN_POINT('Ctrl Pts',(208.562910255543,89.8022376084047,339.539344956919));
#27517=CARTESIAN_POINT('Ctrl Pts',(208.369989533667,89.7397376084047,341.826490424806));
#27518=CARTESIAN_POINT('Ctrl Pts',(206.616317913094,89.6772376084047,343.30733094404));
#27519=CARTESIAN_POINT('Ctrl Pts',(204.86264629252,89.6147376084047,344.788171463274));
#27520=CARTESIAN_POINT('Ctrl Pts',(202.575500824633,89.5522376084047,344.595250741398));
#27521=CARTESIAN_POINT('Ctrl Pts',(200.288355356745,89.4897376084047,344.402330019522));
#27522=CARTESIAN_POINT('Ctrl Pts',(198.807514837511,89.4272376084047,342.648658398949));
#27523=CARTESIAN_POINT('Ctrl Pts',(197.326674318278,89.3647376084047,340.894986778376));
#27524=CARTESIAN_POINT('Ctrl Pts',(197.519595040153,89.3022376084047,338.607841310488));
#27525=CARTESIAN_POINT('Ctrl Pts',(198.05894559721,98.9897376097703,338.653335530367));
#27526=CARTESIAN_POINT('Ctrl Pts',(198.233021996202,98.9272376097703,336.589596378086));
#27527=CARTESIAN_POINT('Ctrl Pts',(199.815396547552,98.8647376097703,335.253403031079));
#27528=CARTESIAN_POINT('Ctrl Pts',(201.397771098903,98.8022376097702,333.917209684073));
#27529=CARTESIAN_POINT('Ctrl Pts',(203.461510251184,98.7397376097702,334.091286083065));
#27530=CARTESIAN_POINT('Ctrl Pts',(205.525249403466,98.6772376097703,334.265362482058));
#27531=CARTESIAN_POINT('Ctrl Pts',(206.861442750472,98.6147376097703,335.847737033408));
#27532=CARTESIAN_POINT('Ctrl Pts',(208.197636097478,98.5522376097703,337.430111584758));
#27533=CARTESIAN_POINT('Ctrl Pts',(208.023559698486,98.4897376097702,339.49385073704));
#27534=CARTESIAN_POINT('Ctrl Pts',(207.849483299494,98.4272376097702,341.557589889321));
#27535=CARTESIAN_POINT('Ctrl Pts',(206.267108748143,98.3647376097703,342.893783236327));
#27536=CARTESIAN_POINT('Ctrl Pts',(204.684734196793,98.3022376097703,344.229976583334));
#27537=CARTESIAN_POINT('Ctrl Pts',(202.620995044512,98.2397376097703,344.055900184342));
#27538=CARTESIAN_POINT('Ctrl Pts',(200.55725589223,98.1772376097702,343.881823785349));
#27539=CARTESIAN_POINT('Ctrl Pts',(199.221062545224,98.1147376097702,342.299449233999));
#27540=CARTESIAN_POINT('Ctrl Pts',(197.884869198218,98.0522376097703,340.717074682649));
#27541=CARTESIAN_POINT('Ctrl Pts',(198.05894559721,97.9897376097703,338.653335530367));
#27542=CARTESIAN_POINT('Ctrl Pts',(198.233021996202,97.9272376097703,336.589596378086));
#27543=CARTESIAN_POINT('Ctrl Pts',(199.815396547552,97.8647376097702,335.253403031079));
#27544=CARTESIAN_POINT('Ctrl Pts',(201.397771098903,97.8022376097703,333.917209684073));
#27545=CARTESIAN_POINT('Ctrl Pts',(203.461510251184,97.7397376097703,334.091286083065));
#27546=CARTESIAN_POINT('Ctrl Pts',(205.525249403466,97.6772376097703,334.265362482058));
#27547=CARTESIAN_POINT('Ctrl Pts',(206.861442750472,97.6147376097703,335.847737033408));
#27548=CARTESIAN_POINT('Ctrl Pts',(208.197636097478,97.5522376097702,337.430111584758));
#27549=CARTESIAN_POINT('Ctrl Pts',(208.023559698486,97.4897376097702,339.49385073704));
#27550=CARTESIAN_POINT('Ctrl Pts',(207.849483299494,97.4272376097703,341.557589889321));
#27551=CARTESIAN_POINT('Ctrl Pts',(206.267108748143,97.3647376097703,342.893783236327));
#27552=CARTESIAN_POINT('Ctrl Pts',(204.684734196793,97.3022376097703,344.229976583334));
#27553=CARTESIAN_POINT('Ctrl Pts',(202.620995044512,97.2397376097702,344.055900184342));
#27554=CARTESIAN_POINT('Ctrl Pts',(200.55725589223,97.1772376097702,343.881823785349));
#27555=CARTESIAN_POINT('Ctrl Pts',(199.221062545224,97.1147376097703,342.299449233999));
#27556=CARTESIAN_POINT('Ctrl Pts',(197.884869198218,97.0522376097703,340.717074682649));
#27557=CARTESIAN_POINT('Ctrl Pts',(198.05894559721,96.9897376097703,338.653335530367));
#27558=CARTESIAN_POINT('Ctrl Pts',(198.233021996202,96.9272376097703,336.589596378086));
#27559=CARTESIAN_POINT('Ctrl Pts',(199.815396547552,96.8647376097702,335.253403031079));
#27560=CARTESIAN_POINT('Ctrl Pts',(201.397771098903,96.8022376097703,333.917209684073));
#27561=CARTESIAN_POINT('Ctrl Pts',(203.461510251184,96.7397376097703,334.091286083065));
#27562=CARTESIAN_POINT('Ctrl Pts',(205.525249403466,96.6772376097703,334.265362482058));
#27563=CARTESIAN_POINT('Ctrl Pts',(206.861442750472,96.6147376097702,335.847737033408));
#27564=CARTESIAN_POINT('Ctrl Pts',(208.197636097478,96.5522376097702,337.430111584758));
#27565=CARTESIAN_POINT('Ctrl Pts',(208.023559698486,96.4897376097703,339.49385073704));
#27566=CARTESIAN_POINT('Ctrl Pts',(207.849483299494,96.4272376097703,341.557589889321));
#27567=CARTESIAN_POINT('Ctrl Pts',(206.267108748143,96.3647376097703,342.893783236327));
#27568=CARTESIAN_POINT('Ctrl Pts',(204.684734196793,96.3022376097702,344.229976583334));
#27569=CARTESIAN_POINT('Ctrl Pts',(202.620995044512,96.2397376097702,344.055900184342));
#27570=CARTESIAN_POINT('Ctrl Pts',(200.55725589223,96.1772376097703,343.881823785349));
#27571=CARTESIAN_POINT('Ctrl Pts',(199.221062545224,96.1147376097703,342.299449233999));
#27572=CARTESIAN_POINT('Ctrl Pts',(197.884869198218,96.0522376097703,340.717074682649));
#27573=CARTESIAN_POINT('Ctrl Pts',(198.05894559721,95.9897376097702,338.653335530367));
#27574=CARTESIAN_POINT('Ctrl Pts',(198.233021996202,95.9272376097703,336.589596378086));
#27575=CARTESIAN_POINT('Ctrl Pts',(199.815396547552,95.8647376097703,335.253403031079));
#27576=CARTESIAN_POINT('Ctrl Pts',(201.397771098903,95.8022376097703,333.917209684073));
#27577=CARTESIAN_POINT('Ctrl Pts',(203.461510251184,95.7397376097702,334.091286083065));
#27578=CARTESIAN_POINT('Ctrl Pts',(205.525249403466,95.6772376097702,334.265362482058));
#27579=CARTESIAN_POINT('Ctrl Pts',(206.861442750472,95.6147376097702,335.847737033408));
#27580=CARTESIAN_POINT('Ctrl Pts',(208.197636097478,95.5522376097703,337.430111584758));
#27581=CARTESIAN_POINT('Ctrl Pts',(208.023559698486,95.4897376097703,339.49385073704));
#27582=CARTESIAN_POINT('Ctrl Pts',(207.849483299494,95.4272376097702,341.557589889321));
#27583=CARTESIAN_POINT('Ctrl Pts',(206.267108748143,95.3647376097702,342.893783236327));
#27584=CARTESIAN_POINT('Ctrl Pts',(204.684734196793,95.3022376097702,344.229976583334));
#27585=CARTESIAN_POINT('Ctrl Pts',(202.620995044512,95.2397376097703,344.055900184342));
#27586=CARTESIAN_POINT('Ctrl Pts',(200.55725589223,95.1772376097703,343.881823785349));
#27587=CARTESIAN_POINT('Ctrl Pts',(199.221062545224,95.1147376097702,342.299449233999));
#27588=CARTESIAN_POINT('Ctrl Pts',(197.884869198218,95.0522376097702,340.717074682649));
#27589=CARTESIAN_POINT('Ctrl Pts',(198.05894559721,94.9897376097702,338.653335530367));
#27590=CARTESIAN_POINT('Ctrl Pts',(198.233021996202,94.9272376097703,336.589596378086));
#27591=CARTESIAN_POINT('Ctrl Pts',(199.815396547552,94.8647376097703,335.253403031079));
#27592=CARTESIAN_POINT('Ctrl Pts',(201.397771098903,94.8022376097703,333.917209684073));
#27593=CARTESIAN_POINT('Ctrl Pts',(203.461510251184,94.7397376097702,334.091286083065));
#27594=CARTESIAN_POINT('Ctrl Pts',(205.525249403466,94.6772376097703,334.265362482058));
#27595=CARTESIAN_POINT('Ctrl Pts',(206.861442750472,94.6147376097703,335.847737033408));
#27596=CARTESIAN_POINT('Ctrl Pts',(208.197636097478,94.5522376097703,337.430111584758));
#27597=CARTESIAN_POINT('Ctrl Pts',(208.023559698486,94.4897376097702,339.49385073704));
#27598=CARTESIAN_POINT('Ctrl Pts',(207.849483299494,94.4272376097702,341.557589889321));
#27599=CARTESIAN_POINT('Ctrl Pts',(206.267108748143,94.3647376097702,342.893783236327));
#27600=CARTESIAN_POINT('Ctrl Pts',(204.684734196793,94.3022376097703,344.229976583334));
#27601=CARTESIAN_POINT('Ctrl Pts',(202.620995044512,94.2397376097703,344.055900184342));
#27602=CARTESIAN_POINT('Ctrl Pts',(200.55725589223,94.1772376097702,343.881823785349));
#27603=CARTESIAN_POINT('Ctrl Pts',(199.221062545224,94.1147376097702,342.299449233999));
#27604=CARTESIAN_POINT('Ctrl Pts',(197.884869198218,94.0522376097702,340.717074682649));
#27605=CARTESIAN_POINT('Ctrl Pts',(198.05894559721,93.9897376097703,338.653335530367));
#27606=CARTESIAN_POINT('Ctrl Pts',(198.233021996202,93.9272376097703,336.589596378086));
#27607=CARTESIAN_POINT('Ctrl Pts',(199.815396547552,93.8647376097702,335.253403031079));
#27608=CARTESIAN_POINT('Ctrl Pts',(201.397771098903,93.8022376097703,333.917209684073));
#27609=CARTESIAN_POINT('Ctrl Pts',(203.461510251184,93.7397376097702,334.091286083065));
#27610=CARTESIAN_POINT('Ctrl Pts',(205.525249403466,93.6772376097703,334.265362482058));
#27611=CARTESIAN_POINT('Ctrl Pts',(206.861442750472,93.6147376097702,335.847737033408));
#27612=CARTESIAN_POINT('Ctrl Pts',(208.197636097478,93.5522376097703,337.430111584758));
#27613=CARTESIAN_POINT('Ctrl Pts',(208.023559698486,93.4897376097702,339.49385073704));
#27614=CARTESIAN_POINT('Ctrl Pts',(207.849483299494,93.4272376097703,341.557589889321));
#27615=CARTESIAN_POINT('Ctrl Pts',(206.267108748143,93.3647376097702,342.893783236327));
#27616=CARTESIAN_POINT('Ctrl Pts',(204.684734196793,93.3022376097703,344.229976583334));
#27617=CARTESIAN_POINT('Ctrl Pts',(202.620995044512,93.2397376097702,344.055900184342));
#27618=CARTESIAN_POINT('Ctrl Pts',(200.55725589223,93.1772376097702,343.881823785349));
#27619=CARTESIAN_POINT('Ctrl Pts',(199.221062545224,93.1147376097702,342.299449233999));
#27620=CARTESIAN_POINT('Ctrl Pts',(197.884869198218,93.0522376097703,340.717074682649));
#27621=CARTESIAN_POINT('Ctrl Pts',(198.05894559721,92.9897376097703,338.653335530367));
#27622=CARTESIAN_POINT('Ctrl Pts',(198.233021996202,92.9272376097703,336.589596378086));
#27623=CARTESIAN_POINT('Ctrl Pts',(199.815396547552,92.8647376097702,335.253403031079));
#27624=CARTESIAN_POINT('Ctrl Pts',(201.397771098903,92.8022376097703,333.917209684073));
#27625=CARTESIAN_POINT('Ctrl Pts',(203.461510251184,92.7397376097703,334.091286083065));
#27626=CARTESIAN_POINT('Ctrl Pts',(205.525249403466,92.6772376097703,334.265362482058));
#27627=CARTESIAN_POINT('Ctrl Pts',(206.861442750472,92.6147376097702,335.847737033408));
#27628=CARTESIAN_POINT('Ctrl Pts',(208.197636097478,92.5522376097702,337.430111584758));
#27629=CARTESIAN_POINT('Ctrl Pts',(208.023559698486,92.4897376097702,339.49385073704));
#27630=CARTESIAN_POINT('Ctrl Pts',(207.849483299494,92.4272376097703,341.557589889321));
#27631=CARTESIAN_POINT('Ctrl Pts',(206.267108748143,92.3647376097703,342.893783236327));
#27632=CARTESIAN_POINT('Ctrl Pts',(204.684734196793,92.3022376097702,344.229976583334));
#27633=CARTESIAN_POINT('Ctrl Pts',(202.620995044512,92.2397376097702,344.055900184342));
#27634=CARTESIAN_POINT('Ctrl Pts',(200.55725589223,92.1772376097702,343.881823785349));
#27635=CARTESIAN_POINT('Ctrl Pts',(199.221062545224,92.1147376097703,342.299449233999));
#27636=CARTESIAN_POINT('Ctrl Pts',(197.884869198218,92.0522376097703,340.717074682649));
#27637=CARTESIAN_POINT('Ctrl Pts',(198.05894559721,91.9897376097702,338.653335530367));
#27638=CARTESIAN_POINT('Ctrl Pts',(198.233021996202,91.9272376097703,336.589596378086));
#27639=CARTESIAN_POINT('Ctrl Pts',(199.815396547552,91.8647376097702,335.253403031079));
#27640=CARTESIAN_POINT('Ctrl Pts',(201.397771098903,91.8022376097703,333.917209684073));
#27641=CARTESIAN_POINT('Ctrl Pts',(203.461510251184,91.7397376097703,334.091286083065));
#27642=CARTESIAN_POINT('Ctrl Pts',(205.525249403466,91.6772376097702,334.265362482058));
#27643=CARTESIAN_POINT('Ctrl Pts',(206.861442750472,91.6147376097702,335.847737033408));
#27644=CARTESIAN_POINT('Ctrl Pts',(208.197636097478,91.5522376097703,337.430111584758));
#27645=CARTESIAN_POINT('Ctrl Pts',(208.023559698486,91.4897376097703,339.49385073704));
#27646=CARTESIAN_POINT('Ctrl Pts',(207.849483299494,91.4272376097703,341.557589889321));
#27647=CARTESIAN_POINT('Ctrl Pts',(206.267108748143,91.3647376097702,342.893783236327));
#27648=CARTESIAN_POINT('Ctrl Pts',(204.684734196793,91.3022376097702,344.229976583334));
#27649=CARTESIAN_POINT('Ctrl Pts',(202.620995044512,91.2397376097702,344.055900184342));
#27650=CARTESIAN_POINT('Ctrl Pts',(200.55725589223,91.1772376097703,343.881823785349));
#27651=CARTESIAN_POINT('Ctrl Pts',(199.221062545224,91.1147376097703,342.299449233999));
#27652=CARTESIAN_POINT('Ctrl Pts',(197.884869198218,91.0522376097702,340.717074682649));
#27653=CARTESIAN_POINT('Ctrl Pts',(198.05894559721,90.9897376097702,338.653335530367));
#27654=CARTESIAN_POINT('Ctrl Pts',(198.233021996202,90.9272376097703,336.589596378086));
#27655=CARTESIAN_POINT('Ctrl Pts',(199.815396547552,90.8647376097703,335.253403031079));
#27656=CARTESIAN_POINT('Ctrl Pts',(201.397771098903,90.8022376097703,333.917209684073));
#27657=CARTESIAN_POINT('Ctrl Pts',(203.461510251184,90.7397376097702,334.091286083065));
#27658=CARTESIAN_POINT('Ctrl Pts',(205.525249403466,90.6772376097702,334.265362482058));
#27659=CARTESIAN_POINT('Ctrl Pts',(206.861442750472,90.6147376097702,335.847737033408));
#27660=CARTESIAN_POINT('Ctrl Pts',(208.197636097478,90.5522376097703,337.430111584758));
#27661=CARTESIAN_POINT('Ctrl Pts',(208.023559698486,90.4897376097703,339.49385073704));
#27662=CARTESIAN_POINT('Ctrl Pts',(207.849483299494,90.4272376097703,341.557589889321));
#27663=CARTESIAN_POINT('Ctrl Pts',(206.267108748143,90.3647376097702,342.893783236327));
#27664=CARTESIAN_POINT('Ctrl Pts',(204.684734196793,90.3022376097702,344.229976583334));
#27665=CARTESIAN_POINT('Ctrl Pts',(202.620995044512,90.2397376097703,344.055900184342));
#27666=CARTESIAN_POINT('Ctrl Pts',(200.55725589223,90.1772376097703,343.881823785349));
#27667=CARTESIAN_POINT('Ctrl Pts',(199.221062545224,90.1147376097702,342.299449233999));
#27668=CARTESIAN_POINT('Ctrl Pts',(197.884869198218,90.0522376097702,340.717074682649));
#27669=CARTESIAN_POINT('Ctrl Pts',(198.05894559721,89.9897376097702,338.653335530367));
#27670=CARTESIAN_POINT('Ctrl Pts',(198.233021996202,89.9272376097703,336.589596378086));
#27671=CARTESIAN_POINT('Ctrl Pts',(199.815396547552,89.8647376097703,335.253403031079));
#27672=CARTESIAN_POINT('Ctrl Pts',(201.397771098903,89.8022376097703,333.917209684073));
#27673=CARTESIAN_POINT('Ctrl Pts',(203.461510251184,89.7397376097702,334.091286083065));
#27674=CARTESIAN_POINT('Ctrl Pts',(205.525249403466,89.6772376097703,334.265362482058));
#27675=CARTESIAN_POINT('Ctrl Pts',(206.861442750472,89.6147376097703,335.847737033408));
#27676=CARTESIAN_POINT('Ctrl Pts',(208.197636097478,89.5522376097703,337.430111584758));
#27677=CARTESIAN_POINT('Ctrl Pts',(208.023559698486,89.4897376097702,339.49385073704));
#27678=CARTESIAN_POINT('Ctrl Pts',(207.849483299494,89.4272376097702,341.557589889321));
#27679=CARTESIAN_POINT('Ctrl Pts',(206.267108748143,89.3647376097702,342.893783236327));
#27680=CARTESIAN_POINT('Ctrl Pts',(204.684734196793,89.3022376097703,344.229976583334));
#27681=CARTESIAN_POINT('Ctrl Pts',(202.620995044512,89.2397376097703,344.055900184342));
#27682=CARTESIAN_POINT('Ctrl Pts',(200.55725589223,89.1772376097702,343.881823785349));
#27683=CARTESIAN_POINT('Ctrl Pts',(199.221062545224,89.1147376097702,342.299449233999));
#27684=CARTESIAN_POINT('Ctrl Pts',(197.884869198218,89.0522376097702,340.717074682649));
#27685=CARTESIAN_POINT('Ctrl Pts',(198.05894559721,88.9897376097703,338.653335530367));
#27686=CARTESIAN_POINT('Origin',(198.50948172921,94.0657194375285,329.433708166765));
#27687=CARTESIAN_POINT('Origin',(213.655523378095,94.0657194375285,339.968906877501));
#27688=CARTESIAN_POINT('Origin',(209.123752459458,94.0657194375285,330.329021910562));
#27689=CARTESIAN_POINT('Origin',(192.426981917601,94.0657194375285,338.178279389906));
#27690=CARTESIAN_POINT('Origin',(196.958752836238,94.0657194375285,347.818164356844));
#27691=CARTESIAN_POINT('Origin',(207.573023566486,94.0657194375285,348.713478100642));
#27692=CARTESIAN_POINT('',(0.,0.,0.));
#27693=CARTESIAN_POINT('Origin',(11.0200923794881,112.698833864687,276.073593133701));
#27694=CARTESIAN_POINT('',(2.0828967647605,117.185094506256,276.373593133701));
#27695=CARTESIAN_POINT('Origin',(11.0200923794881,112.698833864687,276.373593133701));
#27696=CARTESIAN_POINT('',(2.35101263320233,117.050506687009,276.073593133701));
#27697=CARTESIAN_POINT('',(2.35101263320233,117.050506687009,276.073593133701));
#27698=CARTESIAN_POINT('Origin',(11.0200923794881,112.698833864687,276.073593133701));
#27699=CARTESIAN_POINT('Origin',(11.0200923794881,112.698833864687,297.473593133701));
#27700=CARTESIAN_POINT('',(5.65777501065156,115.390590249628,297.473593133701));
#27701=CARTESIAN_POINT('',(16.3824097483247,110.007077479745,297.473593133701));
#27702=CARTESIAN_POINT('Origin',(11.0200923794881,112.698833864687,297.473593133701));
#27703=CARTESIAN_POINT('Origin',(11.0200923794881,112.698833864687,297.473593133701));
#27704=CARTESIAN_POINT('',(15.8461780114411,110.276253118239,298.073593133701));
#27705=CARTESIAN_POINT('',(16.3824097483247,110.007077479745,297.473593133701));
#27706=CARTESIAN_POINT('Origin',(11.0200923794881,112.698833864687,298.073593133701));
#27707=CARTESIAN_POINT('Origin',(11.0200923794881,112.698833864687,276.073593133701));
#27708=CARTESIAN_POINT('',(2.0828967647605,117.185094506256,278.073593133701));
#27709=CARTESIAN_POINT('Origin',(11.0200923794881,112.698833864687,278.073593133701));
#27710=CARTESIAN_POINT('',(2.0828967647605,117.185094506256,276.073593133701));
#27711=CARTESIAN_POINT('Origin',(11.0200923794881,112.698833864687,278.073593133701));
#27712=CARTESIAN_POINT('',(5.65777501065155,115.390590249628,278.073593133701));
#27713=CARTESIAN_POINT('',(5.65777501065155,115.390590249628,278.073593133701));
#27714=CARTESIAN_POINT('Origin',(11.0200923794881,112.698833864687,278.073593133701));
#27715=CARTESIAN_POINT('Origin',(11.0200923794881,112.698833864687,298.073593133701));
#27716=CARTESIAN_POINT('Origin',(11.0200923794881,112.698833864687,276.073593133701));
#27717=CARTESIAN_POINT('Origin',(11.0200923794881,112.698833864687,278.073593133701));
#27718=CARTESIAN_POINT('',(0.,0.,0.));
#27719=CARTESIAN_POINT('Origin',(277.041252647846,78.7397376070391,303.073593133701));
#27720=CARTESIAN_POINT('',(283.962238980384,75.8501099173832,302.073593133701));
#27721=CARTESIAN_POINT('Origin',(277.041252647846,78.7397376070391,302.073593133701));
#27722=CARTESIAN_POINT('',(283.039440802712,76.2353936093374,303.073593133701));
#27723=CARTESIAN_POINT('',(283.039440802712,76.2353936093374,303.073593133701));
#27724=CARTESIAN_POINT('Origin',(277.041252647846,78.7397376070391,303.073593133701));
#27725=CARTESIAN_POINT('Origin',(277.041252647846,78.7397376070391,204.073593133701));
#27726=CARTESIAN_POINT('',(283.962238980384,75.8501099173832,204.073593133701));
#27727=CARTESIAN_POINT('',(270.120266315309,81.629365296695,204.073593133701));
#27728=CARTESIAN_POINT('Origin',(277.041252647846,78.7397376070391,204.073593133701));
#27729=CARTESIAN_POINT('Origin',(277.041252647846,78.7397376070391,204.073593133701));
#27730=CARTESIAN_POINT('',(271.04306449298,81.2440816047409,203.073593133701));
#27731=CARTESIAN_POINT('',(270.120266315309,81.629365296695,204.073593133701));
#27732=CARTESIAN_POINT('Origin',(277.041252647846,78.7397376070391,203.073593133701));
#27733=CARTESIAN_POINT('Origin',(277.041252647846,78.7397376070391,303.073593133701));
#27734=CARTESIAN_POINT('',(283.962238980384,75.8501099173832,303.073593133701));
#27735=CARTESIAN_POINT('Origin',(277.041252647846,78.7397376070391,303.073593133701));
#27736=CARTESIAN_POINT('Origin',(277.041252647846,78.7397376070391,203.073593133701));
#27737=CARTESIAN_POINT('',(0.,0.,0.));
#27738=CARTESIAN_POINT('',(0.,0.,0.));
#27739=CARTESIAN_POINT('',(0.,0.,0.));
#27740=CARTESIAN_POINT('',(0.,0.,0.));
#27741=CARTESIAN_POINT('',(-5.32907051820075E-14,3.5527136788005E-14,-56.5));
#27742=CARTESIAN_POINT('',(0.,0.,0.));
#27743=CARTESIAN_POINT('',(0.,0.,0.));
#27744=CARTESIAN_POINT('',(0.,0.,0.));
#27745=CARTESIAN_POINT('',(0.,0.,0.));
#27746=CARTESIAN_POINT('',(-44.0433179893517,3.45012907132514E-9,-141.394714061189));
#27747=CARTESIAN_POINT('',(0.,0.,0.));
#27748=CARTESIAN_POINT('',(0.,225.397667728952,506.147186267401));
#27749=CARTESIAN_POINT('',(0.,0.,0.));
#27750=UNCERTAINTY_MEASURE_WITH_UNIT(LENGTH_MEASURE(0.01),#27808,
'DISTANCE_ACCURACY_VALUE',
'Maximum model space distance between geometric entities at asserted c
onnectivities');
#27751=UNCERTAINTY_MEASURE_WITH_UNIT(LENGTH_MEASURE(0.01),#27808,
'DISTANCE_ACCURACY_VALUE',
'Maximum model space distance between geometric entities at asserted c
onnectivities');
#27752=UNCERTAINTY_MEASURE_WITH_UNIT(LENGTH_MEASURE(0.01),#27808,
'DISTANCE_ACCURACY_VALUE',
'Maximum model space distance between geometric entities at asserted c
onnectivities');
#27753=UNCERTAINTY_MEASURE_WITH_UNIT(LENGTH_MEASURE(0.01),#27808,
'DISTANCE_ACCURACY_VALUE',
'Maximum model space distance between geometric entities at asserted c
onnectivities');
#27754=UNCERTAINTY_MEASURE_WITH_UNIT(LENGTH_MEASURE(0.01),#27808,
'DISTANCE_ACCURACY_VALUE',
'Maximum model space distance between geometric entities at asserted c
onnectivities');
#27755=UNCERTAINTY_MEASURE_WITH_UNIT(LENGTH_MEASURE(0.01),#27808,
'DISTANCE_ACCURACY_VALUE',
'Maximum model space distance between geometric entities at asserted c
onnectivities');
#27756=UNCERTAINTY_MEASURE_WITH_UNIT(LENGTH_MEASURE(0.01),#27808,
'DISTANCE_ACCURACY_VALUE',
'Maximum model space distance between geometric entities at asserted c
onnectivities');
#27757=UNCERTAINTY_MEASURE_WITH_UNIT(LENGTH_MEASURE(0.01),#27808,
'DISTANCE_ACCURACY_VALUE',
'Maximum model space distance between geometric entities at asserted c
onnectivities');
#27758=UNCERTAINTY_MEASURE_WITH_UNIT(LENGTH_MEASURE(0.01),#27808,
'DISTANCE_ACCURACY_VALUE',
'Maximum model space distance between geometric entities at asserted c
onnectivities');
#27759=UNCERTAINTY_MEASURE_WITH_UNIT(LENGTH_MEASURE(0.01),#27808,
'DISTANCE_ACCURACY_VALUE',
'Maximum model space distance between geometric entities at asserted c
onnectivities');
#27760=UNCERTAINTY_MEASURE_WITH_UNIT(LENGTH_MEASURE(0.01),#27808,
'DISTANCE_ACCURACY_VALUE',
'Maximum model space distance between geometric entities at asserted c
onnectivities');
#27761=UNCERTAINTY_MEASURE_WITH_UNIT(LENGTH_MEASURE(0.01),#27808,
'DISTANCE_ACCURACY_VALUE',
'Maximum model space distance between geometric entities at asserted c
onnectivities');
#27762=UNCERTAINTY_MEASURE_WITH_UNIT(LENGTH_MEASURE(0.01),#27808,
'DISTANCE_ACCURACY_VALUE',
'Maximum model space distance between geometric entities at asserted c
onnectivities');
#27763=UNCERTAINTY_MEASURE_WITH_UNIT(LENGTH_MEASURE(0.01),#27808,
'DISTANCE_ACCURACY_VALUE',
'Maximum model space distance between geometric entities at asserted c
onnectivities');
#27764=UNCERTAINTY_MEASURE_WITH_UNIT(LENGTH_MEASURE(0.01),#27808,
'DISTANCE_ACCURACY_VALUE',
'Maximum model space distance between geometric entities at asserted c
onnectivities');
#27765=UNCERTAINTY_MEASURE_WITH_UNIT(LENGTH_MEASURE(0.01),#27808,
'DISTANCE_ACCURACY_VALUE',
'Maximum model space distance between geometric entities at asserted c
onnectivities');
#27766=UNCERTAINTY_MEASURE_WITH_UNIT(LENGTH_MEASURE(0.01),#27808,
'DISTANCE_ACCURACY_VALUE',
'Maximum model space distance between geometric entities at asserted c
onnectivities');
#27767=UNCERTAINTY_MEASURE_WITH_UNIT(LENGTH_MEASURE(0.01),#27808,
'DISTANCE_ACCURACY_VALUE',
'Maximum model space distance between geometric entities at asserted c
onnectivities');
#27768=UNCERTAINTY_MEASURE_WITH_UNIT(LENGTH_MEASURE(0.01),#27808,
'DISTANCE_ACCURACY_VALUE',
'Maximum model space distance between geometric entities at asserted c
onnectivities');
#27769=UNCERTAINTY_MEASURE_WITH_UNIT(LENGTH_MEASURE(0.01),#27808,
'DISTANCE_ACCURACY_VALUE',
'Maximum model space distance between geometric entities at asserted c
onnectivities');
#27770=UNCERTAINTY_MEASURE_WITH_UNIT(LENGTH_MEASURE(0.01),#27808,
'DISTANCE_ACCURACY_VALUE',
'Maximum model space distance between geometric entities at asserted c
onnectivities');
#27771=UNCERTAINTY_MEASURE_WITH_UNIT(LENGTH_MEASURE(0.01),#27808,
'DISTANCE_ACCURACY_VALUE',
'Maximum model space distance between geometric entities at asserted c
onnectivities');
#27772=UNCERTAINTY_MEASURE_WITH_UNIT(LENGTH_MEASURE(0.01),#27808,
'DISTANCE_ACCURACY_VALUE',
'Maximum model space distance between geometric entities at asserted c
onnectivities');
#27773=UNCERTAINTY_MEASURE_WITH_UNIT(LENGTH_MEASURE(0.01),#27808,
'DISTANCE_ACCURACY_VALUE',
'Maximum model space distance between geometric entities at asserted c
onnectivities');
#27774=UNCERTAINTY_MEASURE_WITH_UNIT(LENGTH_MEASURE(0.01),#27808,
'DISTANCE_ACCURACY_VALUE',
'Maximum model space distance between geometric entities at asserted c
onnectivities');
#27775=UNCERTAINTY_MEASURE_WITH_UNIT(LENGTH_MEASURE(0.01),#27808,
'DISTANCE_ACCURACY_VALUE',
'Maximum model space distance between geometric entities at asserted c
onnectivities');
#27776=UNCERTAINTY_MEASURE_WITH_UNIT(LENGTH_MEASURE(0.01),#27808,
'DISTANCE_ACCURACY_VALUE',
'Maximum model space distance between geometric entities at asserted c
onnectivities');
#27777=UNCERTAINTY_MEASURE_WITH_UNIT(LENGTH_MEASURE(0.01),#27808,
'DISTANCE_ACCURACY_VALUE',
'Maximum model space distance between geometric entities at asserted c
onnectivities');
#27778=UNCERTAINTY_MEASURE_WITH_UNIT(LENGTH_MEASURE(0.01),#27808,
'DISTANCE_ACCURACY_VALUE',
'Maximum model space distance between geometric entities at asserted c
onnectivities');
#27779=(
GEOMETRIC_REPRESENTATION_CONTEXT(3)
GLOBAL_UNCERTAINTY_ASSIGNED_CONTEXT((#27750))
GLOBAL_UNIT_ASSIGNED_CONTEXT((#27808,#27810,#27811))
REPRESENTATION_CONTEXT('','3D')
);
#27780=(
GEOMETRIC_REPRESENTATION_CONTEXT(3)
GLOBAL_UNCERTAINTY_ASSIGNED_CONTEXT((#27751))
GLOBAL_UNIT_ASSIGNED_CONTEXT((#27808,#27810,#27811))
REPRESENTATION_CONTEXT('','3D')
);
#27781=(
GEOMETRIC_REPRESENTATION_CONTEXT(3)
GLOBAL_UNCERTAINTY_ASSIGNED_CONTEXT((#27752))
GLOBAL_UNIT_ASSIGNED_CONTEXT((#27808,#27810,#27811))
REPRESENTATION_CONTEXT('','3D')
);
#27782=(
GEOMETRIC_REPRESENTATION_CONTEXT(3)
GLOBAL_UNCERTAINTY_ASSIGNED_CONTEXT((#27753))
GLOBAL_UNIT_ASSIGNED_CONTEXT((#27808,#27810,#27811))
REPRESENTATION_CONTEXT('','3D')
);
#27783=(
GEOMETRIC_REPRESENTATION_CONTEXT(3)
GLOBAL_UNCERTAINTY_ASSIGNED_CONTEXT((#27754))
GLOBAL_UNIT_ASSIGNED_CONTEXT((#27808,#27810,#27811))
REPRESENTATION_CONTEXT('','3D')
);
#27784=(
GEOMETRIC_REPRESENTATION_CONTEXT(3)
GLOBAL_UNCERTAINTY_ASSIGNED_CONTEXT((#27755))
GLOBAL_UNIT_ASSIGNED_CONTEXT((#27808,#27810,#27811))
REPRESENTATION_CONTEXT('','3D')
);
#27785=(
GEOMETRIC_REPRESENTATION_CONTEXT(3)
GLOBAL_UNCERTAINTY_ASSIGNED_CONTEXT((#27756))
GLOBAL_UNIT_ASSIGNED_CONTEXT((#27808,#27810,#27811))
REPRESENTATION_CONTEXT('','3D')
);
#27786=(
GEOMETRIC_REPRESENTATION_CONTEXT(3)
GLOBAL_UNCERTAINTY_ASSIGNED_CONTEXT((#27757))
GLOBAL_UNIT_ASSIGNED_CONTEXT((#27808,#27810,#27811))
REPRESENTATION_CONTEXT('','3D')
);
#27787=(
GEOMETRIC_REPRESENTATION_CONTEXT(3)
GLOBAL_UNCERTAINTY_ASSIGNED_CONTEXT((#27758))
GLOBAL_UNIT_ASSIGNED_CONTEXT((#27808,#27810,#27811))
REPRESENTATION_CONTEXT('','3D')
);
#27788=(
GEOMETRIC_REPRESENTATION_CONTEXT(3)
GLOBAL_UNCERTAINTY_ASSIGNED_CONTEXT((#27759))
GLOBAL_UNIT_ASSIGNED_CONTEXT((#27808,#27810,#27811))
REPRESENTATION_CONTEXT('','3D')
);
#27789=(
GEOMETRIC_REPRESENTATION_CONTEXT(3)
GLOBAL_UNCERTAINTY_ASSIGNED_CONTEXT((#27760))
GLOBAL_UNIT_ASSIGNED_CONTEXT((#27808,#27810,#27811))
REPRESENTATION_CONTEXT('','3D')
);
#27790=(
GEOMETRIC_REPRESENTATION_CONTEXT(3)
GLOBAL_UNCERTAINTY_ASSIGNED_CONTEXT((#27761))
GLOBAL_UNIT_ASSIGNED_CONTEXT((#27808,#27810,#27811))
REPRESENTATION_CONTEXT('','3D')
);
#27791=(
GEOMETRIC_REPRESENTATION_CONTEXT(3)
GLOBAL_UNCERTAINTY_ASSIGNED_CONTEXT((#27762))
GLOBAL_UNIT_ASSIGNED_CONTEXT((#27808,#27810,#27811))
REPRESENTATION_CONTEXT('','3D')
);
#27792=(
GEOMETRIC_REPRESENTATION_CONTEXT(3)
GLOBAL_UNCERTAINTY_ASSIGNED_CONTEXT((#27763))
GLOBAL_UNIT_ASSIGNED_CONTEXT((#27808,#27810,#27811))
REPRESENTATION_CONTEXT('','3D')
);
#27793=(
GEOMETRIC_REPRESENTATION_CONTEXT(3)
GLOBAL_UNCERTAINTY_ASSIGNED_CONTEXT((#27764))
GLOBAL_UNIT_ASSIGNED_CONTEXT((#27808,#27810,#27811))
REPRESENTATION_CONTEXT('','3D')
);
#27794=(
GEOMETRIC_REPRESENTATION_CONTEXT(3)
GLOBAL_UNCERTAINTY_ASSIGNED_CONTEXT((#27765))
GLOBAL_UNIT_ASSIGNED_CONTEXT((#27808,#27810,#27811))
REPRESENTATION_CONTEXT('','3D')
);
#27795=(
GEOMETRIC_REPRESENTATION_CONTEXT(3)
GLOBAL_UNCERTAINTY_ASSIGNED_CONTEXT((#27766))
GLOBAL_UNIT_ASSIGNED_CONTEXT((#27808,#27810,#27811))
REPRESENTATION_CONTEXT('','3D')
);
#27796=(
GEOMETRIC_REPRESENTATION_CONTEXT(3)
GLOBAL_UNCERTAINTY_ASSIGNED_CONTEXT((#27767))
GLOBAL_UNIT_ASSIGNED_CONTEXT((#27808,#27810,#27811))
REPRESENTATION_CONTEXT('','3D')
);
#27797=(
GEOMETRIC_REPRESENTATION_CONTEXT(3)
GLOBAL_UNCERTAINTY_ASSIGNED_CONTEXT((#27768))
GLOBAL_UNIT_ASSIGNED_CONTEXT((#27808,#27810,#27811))
REPRESENTATION_CONTEXT('','3D')
);
#27798=(
GEOMETRIC_REPRESENTATION_CONTEXT(3)
GLOBAL_UNCERTAINTY_ASSIGNED_CONTEXT((#27769))
GLOBAL_UNIT_ASSIGNED_CONTEXT((#27808,#27810,#27811))
REPRESENTATION_CONTEXT('','3D')
);
#27799=(
GEOMETRIC_REPRESENTATION_CONTEXT(3)
GLOBAL_UNCERTAINTY_ASSIGNED_CONTEXT((#27770))
GLOBAL_UNIT_ASSIGNED_CONTEXT((#27808,#27810,#27811))
REPRESENTATION_CONTEXT('','3D')
);
#27800=(
GEOMETRIC_REPRESENTATION_CONTEXT(3)
GLOBAL_UNCERTAINTY_ASSIGNED_CONTEXT((#27771))
GLOBAL_UNIT_ASSIGNED_CONTEXT((#27808,#27810,#27811))
REPRESENTATION_CONTEXT('','3D')
);
#27801=(
GEOMETRIC_REPRESENTATION_CONTEXT(3)
GLOBAL_UNCERTAINTY_ASSIGNED_CONTEXT((#27772))
GLOBAL_UNIT_ASSIGNED_CONTEXT((#27808,#27810,#27811))
REPRESENTATION_CONTEXT('','3D')
);
#27802=(
GEOMETRIC_REPRESENTATION_CONTEXT(3)
GLOBAL_UNCERTAINTY_ASSIGNED_CONTEXT((#27773))
GLOBAL_UNIT_ASSIGNED_CONTEXT((#27808,#27810,#27811))
REPRESENTATION_CONTEXT('','3D')
);
#27803=(
GEOMETRIC_REPRESENTATION_CONTEXT(3)
GLOBAL_UNCERTAINTY_ASSIGNED_CONTEXT((#27774))
GLOBAL_UNIT_ASSIGNED_CONTEXT((#27808,#27810,#27811))
REPRESENTATION_CONTEXT('','3D')
);
#27804=(
GEOMETRIC_REPRESENTATION_CONTEXT(3)
GLOBAL_UNCERTAINTY_ASSIGNED_CONTEXT((#27775))
GLOBAL_UNIT_ASSIGNED_CONTEXT((#27808,#27810,#27811))
REPRESENTATION_CONTEXT('','3D')
);
#27805=(
GEOMETRIC_REPRESENTATION_CONTEXT(3)
GLOBAL_UNCERTAINTY_ASSIGNED_CONTEXT((#27776))
GLOBAL_UNIT_ASSIGNED_CONTEXT((#27808,#27810,#27811))
REPRESENTATION_CONTEXT('','3D')
);
#27806=(
GEOMETRIC_REPRESENTATION_CONTEXT(3)
GLOBAL_UNCERTAINTY_ASSIGNED_CONTEXT((#27777))
GLOBAL_UNIT_ASSIGNED_CONTEXT((#27808,#27810,#27811))
REPRESENTATION_CONTEXT('','3D')
);
#27807=(
GEOMETRIC_REPRESENTATION_CONTEXT(3)
GLOBAL_UNCERTAINTY_ASSIGNED_CONTEXT((#27778))
GLOBAL_UNIT_ASSIGNED_CONTEXT((#27808,#27810,#27811))
REPRESENTATION_CONTEXT('','3D')
);
#27808=(
LENGTH_UNIT()
NAMED_UNIT(*)
SI_UNIT(.MILLI.,.METRE.)
);
#27809=(
LENGTH_UNIT()
NAMED_UNIT(*)
SI_UNIT($,.METRE.)
);
#27810=(
NAMED_UNIT(*)
PLANE_ANGLE_UNIT()
SI_UNIT($,.RADIAN.)
);
#27811=(
NAMED_UNIT(*)
SI_UNIT($,.STERADIAN.)
SOLID_ANGLE_UNIT()
);
#27812=SHAPE_DEFINITION_REPRESENTATION(#27840,#27899);
#27813=SHAPE_DEFINITION_REPRESENTATION(#27841,#27900);
#27814=SHAPE_DEFINITION_REPRESENTATION(#27842,#27901);
#27815=SHAPE_DEFINITION_REPRESENTATION(#27843,#27902);
#27816=SHAPE_DEFINITION_REPRESENTATION(#27844,#27903);
#27817=SHAPE_DEFINITION_REPRESENTATION(#27847,#27904);
#27818=SHAPE_DEFINITION_REPRESENTATION(#27848,#27905);
#27819=SHAPE_DEFINITION_REPRESENTATION(#27849,#27906);
#27820=SHAPE_DEFINITION_REPRESENTATION(#27850,#27907);
#27821=SHAPE_DEFINITION_REPRESENTATION(#27854,#27908);
#27822=SHAPE_DEFINITION_REPRESENTATION(#27855,#27909);
#27823=SHAPE_DEFINITION_REPRESENTATION(#27856,#27910);
#27824=SHAPE_DEFINITION_REPRESENTATION(#27857,#27911);
#27825=SHAPE_DEFINITION_REPRESENTATION(#27858,#27912);
#27826=SHAPE_DEFINITION_REPRESENTATION(#27859,#27913);
#27827=SHAPE_DEFINITION_REPRESENTATION(#27860,#27914);
#27828=SHAPE_DEFINITION_REPRESENTATION(#27861,#27915);
#27829=SHAPE_DEFINITION_REPRESENTATION(#27862,#27916);
#27830=SHAPE_DEFINITION_REPRESENTATION(#27870,#27917);
#27831=SHAPE_DEFINITION_REPRESENTATION(#27871,#27918);
#27832=SHAPE_DEFINITION_REPRESENTATION(#27872,#27919);
#27833=SHAPE_DEFINITION_REPRESENTATION(#27873,#27920);
#27834=SHAPE_DEFINITION_REPRESENTATION(#27877,#27921);
#27835=SHAPE_DEFINITION_REPRESENTATION(#27878,#27922);
#27836=SHAPE_DEFINITION_REPRESENTATION(#27879,#27923);
#27837=SHAPE_DEFINITION_REPRESENTATION(#27883,#27924);
#27838=SHAPE_DEFINITION_REPRESENTATION(#27884,#27925);
#27839=SHAPE_DEFINITION_REPRESENTATION(#27885,#27926);
#27840=PRODUCT_DEFINITION_SHAPE('',$,#27928);
#27841=PRODUCT_DEFINITION_SHAPE('',$,#27929);
#27842=PRODUCT_DEFINITION_SHAPE('',$,#27930);
#27843=PRODUCT_DEFINITION_SHAPE('',$,#27931);
#27844=PRODUCT_DEFINITION_SHAPE('',$,#27932);
#27845=PRODUCT_DEFINITION_SHAPE($,$,#175);
#27846=PRODUCT_DEFINITION_SHAPE($,$,#176);
#27847=PRODUCT_DEFINITION_SHAPE('',$,#27933);
#27848=PRODUCT_DEFINITION_SHAPE('',$,#27934);
#27849=PRODUCT_DEFINITION_SHAPE('',$,#27935);
#27850=PRODUCT_DEFINITION_SHAPE('',$,#27936);
#27851=PRODUCT_DEFINITION_SHAPE($,$,#177);
#27852=PRODUCT_DEFINITION_SHAPE($,$,#178);
#27853=PRODUCT_DEFINITION_SHAPE($,$,#179);
#27854=PRODUCT_DEFINITION_SHAPE('',$,#27937);
#27855=PRODUCT_DEFINITION_SHAPE('',$,#27938);
#27856=PRODUCT_DEFINITION_SHAPE('',$,#27939);
#27857=PRODUCT_DEFINITION_SHAPE('',$,#27940);
#27858=PRODUCT_DEFINITION_SHAPE('',$,#27941);
#27859=PRODUCT_DEFINITION_SHAPE('',$,#27942);
#27860=PRODUCT_DEFINITION_SHAPE('',$,#27943);
#27861=PRODUCT_DEFINITION_SHAPE('',$,#27944);
#27862=PRODUCT_DEFINITION_SHAPE('',$,#27945);
#27863=PRODUCT_DEFINITION_SHAPE($,$,#180);
#27864=PRODUCT_DEFINITION_SHAPE($,$,#181);
#27865=PRODUCT_DEFINITION_SHAPE($,$,#182);
#27866=PRODUCT_DEFINITION_SHAPE($,$,#183);
#27867=PRODUCT_DEFINITION_SHAPE($,$,#184);
#27868=PRODUCT_DEFINITION_SHAPE($,$,#185);
#27869=PRODUCT_DEFINITION_SHAPE($,$,#186);
#27870=PRODUCT_DEFINITION_SHAPE('',$,#27946);
#27871=PRODUCT_DEFINITION_SHAPE('',$,#27947);
#27872=PRODUCT_DEFINITION_SHAPE('',$,#27948);
#27873=PRODUCT_DEFINITION_SHAPE('',$,#27949);
#27874=PRODUCT_DEFINITION_SHAPE($,$,#187);
#27875=PRODUCT_DEFINITION_SHAPE($,$,#188);
#27876=PRODUCT_DEFINITION_SHAPE($,$,#189);
#27877=PRODUCT_DEFINITION_SHAPE('',$,#27950);
#27878=PRODUCT_DEFINITION_SHAPE('',$,#27951);
#27879=PRODUCT_DEFINITION_SHAPE('',$,#27952);
#27880=PRODUCT_DEFINITION_SHAPE($,$,#190);
#27881=PRODUCT_DEFINITION_SHAPE($,$,#191);
#27882=PRODUCT_DEFINITION_SHAPE($,$,#192);
#27883=PRODUCT_DEFINITION_SHAPE('',$,#27953);
#27884=PRODUCT_DEFINITION_SHAPE('',$,#27954);
#27885=PRODUCT_DEFINITION_SHAPE('',$,#27955);
#27886=PRODUCT_DEFINITION_SHAPE($,$,#193);
#27887=PRODUCT_DEFINITION_SHAPE($,$,#194);
#27888=PRODUCT_DEFINITION_SHAPE($,$,#195);
#27889=PRODUCT_DEFINITION_SHAPE($,$,#196);
#27890=PRODUCT_DEFINITION_SHAPE($,$,#197);
#27891=PRODUCT_DEFINITION_SHAPE($,$,#198);
#27892=PRODUCT_DEFINITION_SHAPE($,$,#199);
#27893=PRODUCT_DEFINITION_SHAPE($,$,#200);
#27894=PRODUCT_DEFINITION_SHAPE($,$,#201);
#27895=PRODUCT_DEFINITION_SHAPE($,$,#202);
#27896=PRODUCT_DEFINITION_SHAPE($,$,#203);
#27897=PRODUCT_DEFINITION_SHAPE($,$,#204);
#27898=PRODUCT_DEFINITION_SHAPE($,$,#205);
#27899=SHAPE_REPRESENTATION('',(#12298,#13719,#13720,#13721,#13722,#13723,
#13724,#13725,#13726,#13727,#13728,#13729,#13730,#13731),#27779);
#27900=SHAPE_REPRESENTATION('',(#12299),#27780);
#27901=SHAPE_REPRESENTATION('',(#12652,#12782,#12783),#27781);
#27902=SHAPE_REPRESENTATION('',(#12653),#27782);
#27903=SHAPE_REPRESENTATION('',(#12749),#27783);
#27904=SHAPE_REPRESENTATION('',(#12784,#12965,#12966,#12967),#27784);
#27905=SHAPE_REPRESENTATION('',(#12785),#27785);
#27906=SHAPE_REPRESENTATION('',(#12859),#27786);
#27907=SHAPE_REPRESENTATION('',(#12944),#27787);
#27908=SHAPE_REPRESENTATION('',(#12968),#27788);
#27909=SHAPE_REPRESENTATION('',(#12993,#13361,#13362,#13363,#13364,#13365,
#13366,#13367),#27789);
#27910=SHAPE_REPRESENTATION('',(#12994),#27790);
#27911=SHAPE_REPRESENTATION('',(#13164),#27791);
#27912=SHAPE_REPRESENTATION('',(#13186),#27792);
#27913=SHAPE_REPRESENTATION('',(#13208),#27793);
#27914=SHAPE_REPRESENTATION('',(#13212),#27794);
#27915=SHAPE_REPRESENTATION('',(#13263),#27795);
#27916=SHAPE_REPRESENTATION('',(#13302),#27796);
#27917=SHAPE_REPRESENTATION('',(#13368,#13452,#13453,#13454),#27797);
#27918=SHAPE_REPRESENTATION('',(#13369),#27798);
#27919=SHAPE_REPRESENTATION('',(#13422),#27799);
#27920=SHAPE_REPRESENTATION('',(#13434),#27800);
#27921=SHAPE_REPRESENTATION('',(#13455,#13512,#13513,#13514),#27801);
#27922=SHAPE_REPRESENTATION('',(#13456),#27802);
#27923=SHAPE_REPRESENTATION('',(#13467),#27803);
#27924=SHAPE_REPRESENTATION('',(#13515),#27804);
#27925=SHAPE_REPRESENTATION('',(#13693),#27805);
#27926=SHAPE_REPRESENTATION('',(#13708),#27806);
#27927=PRODUCT_DEFINITION_CONTEXT('part definition',#28013,'design');
#27928=PRODUCT_DEFINITION('iport MAT-057',
'MAT-057',#27956,#27927);
#27929=PRODUCT_DEFINITION('Main Frame','Main Frame',#27957,#27927);
#27930=PRODUCT_DEFINITION('Lifting Arm Assembly','Lifting Arm Assembly',
#27958,#27927);
#27931=PRODUCT_DEFINITION('Lifting Arm','Lifting Arm',#27959,#27927);
#27932=PRODUCT_DEFINITION('Arm Rollers','Arm Rollers',#27960,#27927);
#27933=PRODUCT_DEFINITION('Saddle Assembly','Saddle Assembly',#27961,#27927);
#27934=PRODUCT_DEFINITION('Lifting Saddle','Lifting Saddle',#27962,#27927);
#27935=PRODUCT_DEFINITION('Saddle Holder','Saddle Holder',#27963,#27927);
#27936=PRODUCT_DEFINITION('Saddle Pins','Saddle Pins',#27964,#27927);
#27937=PRODUCT_DEFINITION('Saddle Link','Saddle Link',#27965,#27927);
#27938=PRODUCT_DEFINITION('Hydraulic Pump Unit','Hydraulic Pump Unit',#27966,
#27927);
#27939=PRODUCT_DEFINITION('Pump Body','Pump Body',#27967,#27927);
#27940=PRODUCT_DEFINITION('Hydraulic Ram','Hydraulic Ram',#27968,#27927);
#27941=PRODUCT_DEFINITION('Release Valve Screw','Release Valve Screw',#27969,
#27927);
#27942=PRODUCT_DEFINITION('Valve Ball','Valve Ball',#27970,#27927);
#27943=PRODUCT_DEFINITION('Valve Fitting','Valve Fitting',#27971,#27927);
#27944=PRODUCT_DEFINITION('Pump Pins','Pump Pins',#27972,#27927);
#27945=PRODUCT_DEFINITION('Retaining Clips','Retaining Clips',#27973,#27927);
#27946=PRODUCT_DEFINITION('Handle Assembly','Handle Assembly',#27974,#27927);
#27947=PRODUCT_DEFINITION('Handle Socket','Handle Socket',#27975,#27927);
#27948=PRODUCT_DEFINITION('Handle Tube','Handle Tube',#27976,#27927);
#27949=PRODUCT_DEFINITION('Handle Grip','Handle Grip',#27977,#27927);
#27950=PRODUCT_DEFINITION('Front Wheel Assembly','Front Wheel Assembly',
#27978,#27927);
#27951=PRODUCT_DEFINITION('Front Axle','Front Axle',#27979,#27927);
#27952=PRODUCT_DEFINITION('Front Wheel','Front Wheel',#27980,#27927);
#27953=PRODUCT_DEFINITION('Rear Caster Wheel','Rear Caster Wheel',#27981,
#27927);
#27954=PRODUCT_DEFINITION('Pivot Pin Cap','Pivot Pin Cap',#27982,#27927);
#27955=PRODUCT_DEFINITION('Handle Pivot Pin','Handle Pivot Pin',#27983,
#27927);
#27956=PRODUCT_DEFINITION_FORMATION('',$,#28015);
#27957=PRODUCT_DEFINITION_FORMATION('',$,#28016);
#27958=PRODUCT_DEFINITION_FORMATION('',$,#28017);
#27959=PRODUCT_DEFINITION_FORMATION('',$,#28018);
#27960=PRODUCT_DEFINITION_FORMATION('',$,#28019);
#27961=PRODUCT_DEFINITION_FORMATION('',$,#28020);
#27962=PRODUCT_DEFINITION_FORMATION('',$,#28021);
#27963=PRODUCT_DEFINITION_FORMATION('',$,#28022);
#27964=PRODUCT_DEFINITION_FORMATION('',$,#28023);
#27965=PRODUCT_DEFINITION_FORMATION('',$,#28024);
#27966=PRODUCT_DEFINITION_FORMATION('',$,#28025);
#27967=PRODUCT_DEFINITION_FORMATION('',$,#28026);
#27968=PRODUCT_DEFINITION_FORMATION('',$,#28027);
#27969=PRODUCT_DEFINITION_FORMATION('',$,#28028);
#27970=PRODUCT_DEFINITION_FORMATION('',$,#28029);
#27971=PRODUCT_DEFINITION_FORMATION('',$,#28030);
#27972=PRODUCT_DEFINITION_FORMATION('',$,#28031);
#27973=PRODUCT_DEFINITION_FORMATION('',$,#28032);
#27974=PRODUCT_DEFINITION_FORMATION('',$,#28033);
#27975=PRODUCT_DEFINITION_FORMATION('',$,#28034);
#27976=PRODUCT_DEFINITION_FORMATION('',$,#28035);
#27977=PRODUCT_DEFINITION_FORMATION('',$,#28036);
#27978=PRODUCT_DEFINITION_FORMATION('',$,#28037);
#27979=PRODUCT_DEFINITION_FORMATION('',$,#28038);
#27980=PRODUCT_DEFINITION_FORMATION('',$,#28039);
#27981=PRODUCT_DEFINITION_FORMATION('',$,#28040);
#27982=PRODUCT_DEFINITION_FORMATION('',$,#28041);
#27983=PRODUCT_DEFINITION_FORMATION('',$,#28042);
#27984=PRODUCT_RELATED_PRODUCT_CATEGORY('MAT-057',
'MAT-057',(#28015));
#27985=PRODUCT_RELATED_PRODUCT_CATEGORY('Main Frame','Main Frame',(#28016));
#27986=PRODUCT_RELATED_PRODUCT_CATEGORY('Lifting Arm Assembly',
'Lifting Arm Assembly',(#28017));
#27987=PRODUCT_RELATED_PRODUCT_CATEGORY('Lifting Arm','Lifting Arm',(#28018));
#27988=PRODUCT_RELATED_PRODUCT_CATEGORY('Arm Rollers','Arm Rollers',(#28019));
#27989=PRODUCT_RELATED_PRODUCT_CATEGORY('Saddle Assembly',
'Saddle Assembly',(#28020));
#27990=PRODUCT_RELATED_PRODUCT_CATEGORY('Lifting Saddle',
'Lifting Saddle',(#28021));
#27991=PRODUCT_RELATED_PRODUCT_CATEGORY('Saddle Holder','Saddle Holder',
(#28022));
#27992=PRODUCT_RELATED_PRODUCT_CATEGORY('Saddle Pins','Saddle Pins',(#28023));
#27993=PRODUCT_RELATED_PRODUCT_CATEGORY('Saddle Link','Saddle Link',(#28024));
#27994=PRODUCT_RELATED_PRODUCT_CATEGORY('Hydraulic Pump Unit',
'Hydraulic Pump Unit',(#28025));
#27995=PRODUCT_RELATED_PRODUCT_CATEGORY('Pump Body','Pump Body',(#28026));
#27996=PRODUCT_RELATED_PRODUCT_CATEGORY('Hydraulic Ram','Hydraulic Ram',
(#28027));
#27997=PRODUCT_RELATED_PRODUCT_CATEGORY('Release Valve Screw',
'Release Valve Screw',(#28028));
#27998=PRODUCT_RELATED_PRODUCT_CATEGORY('Valve Ball','Valve Ball',(#28029));
#27999=PRODUCT_RELATED_PRODUCT_CATEGORY('Valve Fitting','Valve Fitting',
(#28030));
#28000=PRODUCT_RELATED_PRODUCT_CATEGORY('Pump Pins','Pump Pins',(#28031));
#28001=PRODUCT_RELATED_PRODUCT_CATEGORY('Retaining Clips',
'Retaining Clips',(#28032));
#28002=PRODUCT_RELATED_PRODUCT_CATEGORY('Handle Assembly',
'Handle Assembly',(#28033));
#28003=PRODUCT_RELATED_PRODUCT_CATEGORY('Handle Socket','Handle Socket',
(#28034));
#28004=PRODUCT_RELATED_PRODUCT_CATEGORY('Handle Tube','Handle Tube',(#28035));
#28005=PRODUCT_RELATED_PRODUCT_CATEGORY('Handle Grip','Handle Grip',(#28036));
#28006=PRODUCT_RELATED_PRODUCT_CATEGORY('Front Wheel Assembly',
'Front Wheel Assembly',(#28037));
#28007=PRODUCT_RELATED_PRODUCT_CATEGORY('Front Axle','Front Axle',(#28038));
#28008=PRODUCT_RELATED_PRODUCT_CATEGORY('Front Wheel','Front Wheel',(#28039));
#28009=PRODUCT_RELATED_PRODUCT_CATEGORY('Rear Caster Wheel',
'Rear Caster Wheel',(#28040));
#28010=PRODUCT_RELATED_PRODUCT_CATEGORY('Pivot Pin Cap','Pivot Pin Cap',
(#28041));
#28011=PRODUCT_RELATED_PRODUCT_CATEGORY('Handle Pivot Pin',
'Handle Pivot Pin',(#28042));
#28012=APPLICATION_PROTOCOL_DEFINITION('international standard',
'ap242_managed_model_based_3d_engineering',2011,#28013);
#28013=APPLICATION_CONTEXT('Managed model based 3d engineering');
#28014=PRODUCT_CONTEXT('part definition',#28013,'mechanical');
#28015=PRODUCT('iport MAT-057','MAT-057',
'STEP AP214',(#28014));
#28016=PRODUCT('Main Frame','Main Frame',$,(#28014));
#28017=PRODUCT('Lifting Arm Assembly','Lifting Arm Assembly',$,(#28014));
#28018=PRODUCT('Lifting Arm','Lifting Arm',$,(#28014));
#28019=PRODUCT('Arm Rollers','Arm Rollers',$,(#28014));
#28020=PRODUCT('Saddle Assembly','Saddle Assembly',$,(#28014));
#28021=PRODUCT('Lifting Saddle','Lifting Saddle',$,(#28014));
#28022=PRODUCT('Saddle Holder','Saddle Holder',$,(#28014));
#28023=PRODUCT('Saddle Pins','Saddle Pins',$,(#28014));
#28024=PRODUCT('Saddle Link','Saddle Link',$,(#28014));
#28025=PRODUCT('Hydraulic Pump Unit','Hydraulic Pump Unit',$,(#28014));
#28026=PRODUCT('Pump Body','Pump Body',$,(#28014));
#28027=PRODUCT('Hydraulic Ram','Hydraulic Ram',$,(#28014));
#28028=PRODUCT('Release Valve Screw','Release Valve Screw',$,(#28014));
#28029=PRODUCT('Valve Ball','Valve Ball',$,(#28014));
#28030=PRODUCT('Valve Fitting','Valve Fitting',$,(#28014));
#28031=PRODUCT('Pump Pins','Pump Pins',$,(#28014));
#28032=PRODUCT('Retaining Clips','Retaining Clips',$,(#28014));
#28033=PRODUCT('Handle Assembly','Handle Assembly',$,(#28014));
#28034=PRODUCT('Handle Socket','Handle Socket',$,(#28014));
#28035=PRODUCT('Handle Tube','Handle Tube',$,(#28014));
#28036=PRODUCT('Handle Grip','Handle Grip',$,(#28014));
#28037=PRODUCT('Front Wheel Assembly','Front Wheel Assembly',$,(#28014));
#28038=PRODUCT('Front Axle','Front Axle',$,(#28014));
#28039=PRODUCT('Front Wheel','Front Wheel',$,(#28014));
#28040=PRODUCT('Rear Caster Wheel','Rear Caster Wheel',$,(#28014));
#28041=PRODUCT('Pivot Pin Cap','Pivot Pin Cap',$,(#28014));
#28042=PRODUCT('Handle Pivot Pin','Handle Pivot Pin',$,(#28014));
#28043=PRESENTATION_STYLE_ASSIGNMENT((#28044));
#28044=SURFACE_STYLE_USAGE(.BOTH.,#28045);
#28045=SURFACE_SIDE_STYLE('',(#28046));
#28046=SURFACE_STYLE_FILL_AREA(#28047);
#28047=FILL_AREA_STYLE('Steel - Satin',(#28048));
#28048=FILL_AREA_STYLE_COLOUR('Steel - Satin',#28049);
#28049=COLOUR_RGB('Steel - Satin',0.627450980392157,0.627450980392157,0.627450980392157);
#28050=COLOUR_RGB('Dark Blue',0.08,0.2,0.34);
#28051=FILL_AREA_STYLE_COLOUR('',#28050);
#28052=FILL_AREA_STYLE('',(#28051));
#28053=SURFACE_STYLE_FILL_AREA(#28052);
#28054=SURFACE_SIDE_STYLE('',(#28053));
#28055=SURFACE_STYLE_USAGE(.BOTH.,#28054);
#28056=PRESENTATION_STYLE_ASSIGNMENT((#28055));
#28057=COLOUR_RGB('Light Blue',0.38,0.62,0.78);
#28058=FILL_AREA_STYLE_COLOUR('',#28057);
#28059=FILL_AREA_STYLE('',(#28058));
#28060=SURFACE_STYLE_FILL_AREA(#28059);
#28061=SURFACE_SIDE_STYLE('',(#28060));
#28062=SURFACE_STYLE_USAGE(.BOTH.,#28061);
#28063=PRESENTATION_STYLE_ASSIGNMENT((#28062));
#28064=COLOUR_RGB('Sky Blue',0.24,0.69,0.87);
#28065=FILL_AREA_STYLE_COLOUR('',#28064);
#28066=FILL_AREA_STYLE('',(#28065));
#28067=SURFACE_STYLE_FILL_AREA(#28066);
#28068=SURFACE_SIDE_STYLE('',(#28067));
#28069=SURFACE_STYLE_USAGE(.BOTH.,#28068);
#28070=PRESENTATION_STYLE_ASSIGNMENT((#28069));
#28071=COLOUR_RGB('Grey',0.48,0.52,0.57);
#28072=FILL_AREA_STYLE_COLOUR('',#28071);
#28073=FILL_AREA_STYLE('',(#28072));
#28074=SURFACE_STYLE_FILL_AREA(#28073);
#28075=SURFACE_SIDE_STYLE('',(#28074));
#28076=SURFACE_STYLE_USAGE(.BOTH.,#28075);
#28077=PRESENTATION_STYLE_ASSIGNMENT((#28076));
#28078=COLOUR_RGB('Black',0.12,0.14,0.17);
#28079=FILL_AREA_STYLE_COLOUR('',#28078);
#28080=FILL_AREA_STYLE('',(#28079));
#28081=SURFACE_STYLE_FILL_AREA(#28080);
#28082=SURFACE_SIDE_STYLE('',(#28081));
#28083=SURFACE_STYLE_USAGE(.BOTH.,#28082);
#28084=PRESENTATION_STYLE_ASSIGNMENT((#28083));
#28085=COLOUR_RGB('Off White',0.89,0.88,0.83);
#28086=FILL_AREA_STYLE_COLOUR('',#28085);
#28087=FILL_AREA_STYLE('',(#28086));
#28088=SURFACE_STYLE_FILL_AREA(#28087);
#28089=SURFACE_SIDE_STYLE('',(#28088));
#28090=SURFACE_STYLE_USAGE(.BOTH.,#28089);
#28091=PRESENTATION_STYLE_ASSIGNMENT((#28090));
ENDSEC;
END-ISO-10303-21;
